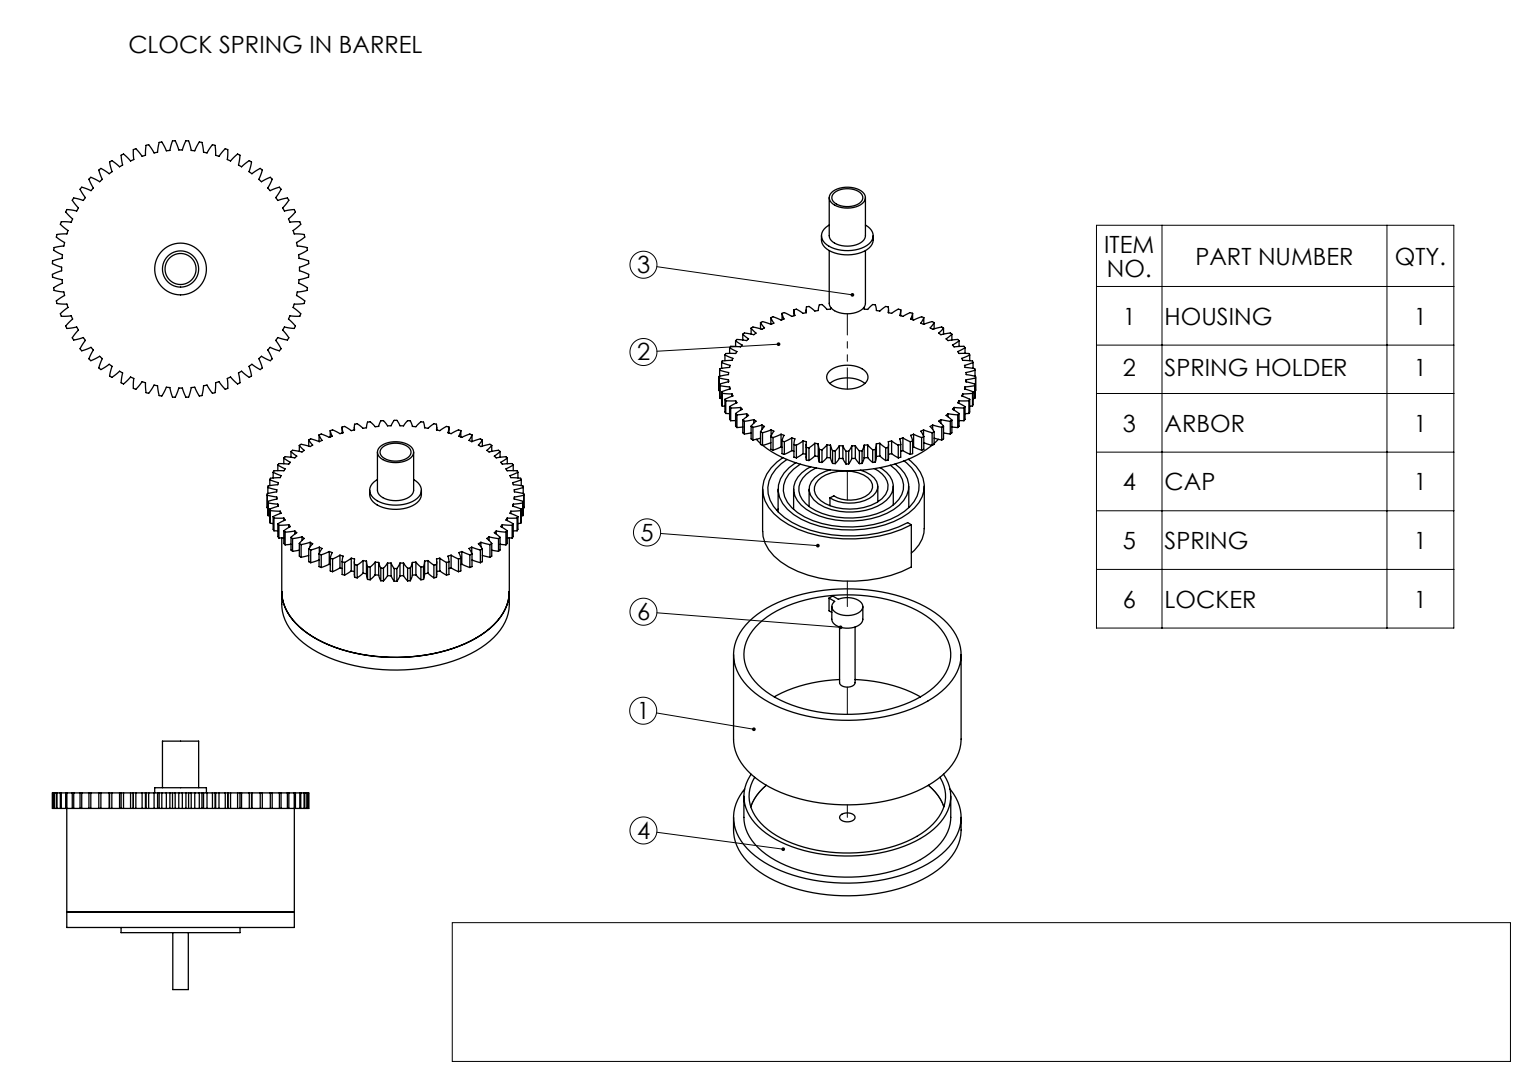
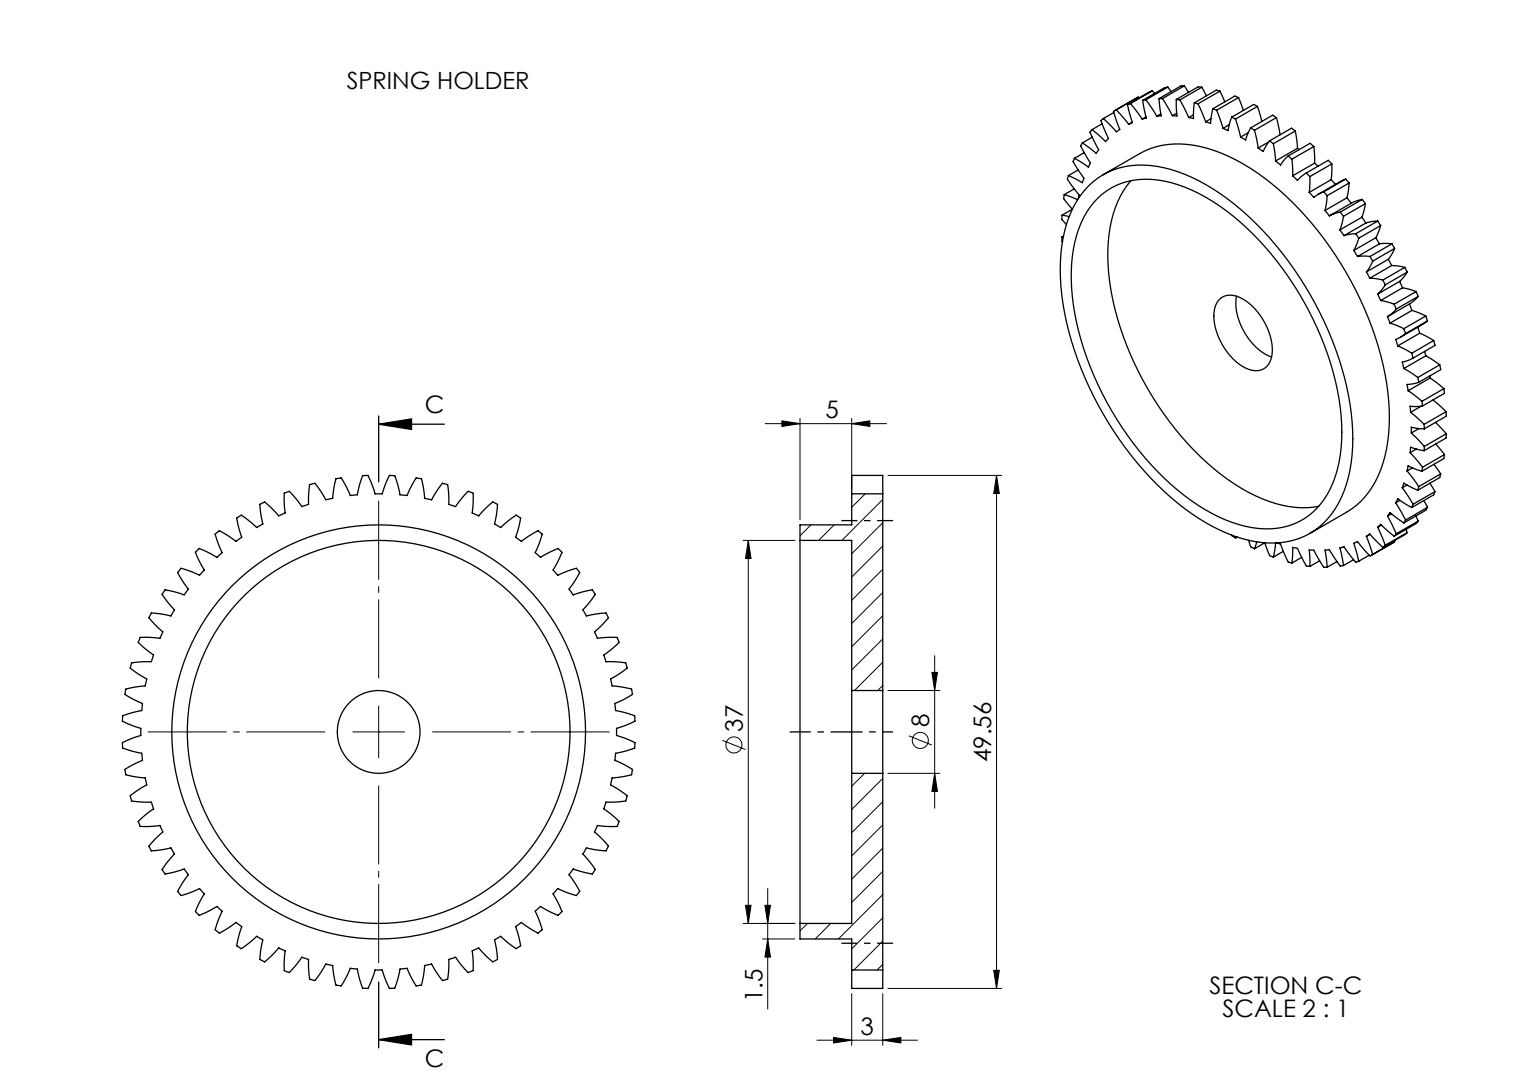
ISO-10303-21;
HEADER;
FILE_DESCRIPTION (('STEP AP214'),
    '1' );
FILE_NAME ('BR-102',
    '2026-10-08T12:30:53',
    ( '' ),
    ( '' ),
    'SwSTEP 2.0',
    'SolidWorks 2026',
    '' );
FILE_SCHEMA (( 'AUTOMOTIVE_DESIGN' ));
ENDSEC;

DATA;
#1 = VECTOR ( 'NONE', #9436, 1000.000000000000000 ) ;
#2 = CARTESIAN_POINT ( 'NONE',  ( 0.000000000000000000, 11.20082935824103565, -20.08719549084853284 ) ) ;
#3 = CIRCLE ( 'NONE', #2554, 9.599999999999994316 ) ;
#4 = ORIENTED_EDGE ( 'NONE', *, *, #1712, .F. ) ;
#5 = CARTESIAN_POINT ( 'NONE',  ( 13.54728169684850414, 0.8932250400876640128, 10.00000000000000000 ) ) ;
#6 = CARTESIAN_POINT ( 'NONE',  ( 3.000000000000000888, -19.29833442572367375, 11.67026512804540950 ) ) ;
#7 = CIRCLE ( 'NONE', #8025, 9.599999999999996092 ) ;
#8 = DIRECTION ( 'NONE',  ( 0.000000000000000000, 0.000000000000000000, 1.000000000000000000 ) ) ;
#9 = AXIS2_PLACEMENT_3D ( 'NONE', #2328, #5147, #7953 ) ;
#10 = DIRECTION ( 'NONE',  ( 0.000000000000000000, 0.000000000000000000, 1.000000000000000000 ) ) ;
#11 = CARTESIAN_POINT ( 'NONE',  ( -13.43906451854578954, -9.301052350413227643, 10.00000000000000000 ) ) ;
#12 = CARTESIAN_POINT ( 'NONE',  ( 8.539395351299290837, 0.2748098766782898217, 6.857782953271941950E-17 ) ) ;
#13 = DIRECTION ( 'NONE',  ( -1.000000000000000000, -0.000000000000000000, -0.000000000000000000 ) ) ;
#14 = CARTESIAN_POINT ( 'NONE',  ( -22.00000000000000000, 0.000000000000000000, 3.000000000000000000 ) ) ;
#15 = EDGE_CURVE ( 'NONE', #3183, #6148, #9804, .T. ) ;
#16 = ORIENTED_EDGE ( 'NONE', *, *, #10840, .T. ) ;
#17 = AXIS2_PLACEMENT_3D ( 'NONE', #6287, #975, #11260 ) ;
#18 = PRODUCT ( 'spring', 'spring', '', ( #10456 ) ) ;
#19 = EDGE_LOOP ( 'NONE', ( #9760, #9661, #8021, #4048 ) ) ;
#20 = AXIS2_PLACEMENT_3D ( 'NONE', #2237, #8791, #3220 ) ;
#21 = MECHANICAL_DESIGN_GEOMETRIC_PRESENTATION_REPRESENTATION (  '', ( #419 ), #8834 ) ;
#22 = ORIENTED_EDGE ( 'NONE', *, *, #6904, .T. ) ;
#23 = CIRCLE ( 'NONE', #4524, 9.599999999999997868 ) ;
#24 = ADVANCED_FACE ( 'NONE', ( #5969 ), #4246, .T. ) ;
#25 = LINE ( 'NONE', #9459, #11094 ) ;
#26 = CARTESIAN_POINT ( 'NONE',  ( 10.50580257846854337, 1.391709641844861123, 10.00000000000000000 ) ) ;
#27 = DIRECTION ( 'NONE',  ( -1.000000000000000000, 0.000000000000000000, -0.000000000000000000 ) ) ;
#28 = DIRECTION ( 'NONE',  ( -1.000000000000000000, 0.000000000000000000, 0.000000000000000000 ) ) ;
#29 = CARTESIAN_POINT ( 'NONE',  ( 3.000000000000000888, 21.14796121233209192, -9.039786367038628256 ) ) ;
#30 = CIRCLE ( 'NONE', #1023, 22.99899999999999878 ) ;
#31 = CARTESIAN_POINT ( 'NONE',  ( 8.800885721068835821, 6.316044917328127895, 3.747395293195558847E-16 ) ) ;
#32 = EDGE_CURVE ( 'NONE', #9019, #7573, #5110, .T. ) ;
#33 = DIRECTION ( 'NONE',  ( 0.000000000000000000, 0.3090169943749479509, -0.9510565162951534202 ) ) ;
#34 = DIRECTION ( 'NONE',  ( 0.000000000000000000, -1.000000000000000000, -1.048062100069321163E-14 ) ) ;
#35 = VERTEX_POINT ( 'NONE', #7865 ) ;
#36 = ORIENTED_EDGE ( 'NONE', *, *, #9803, .F. ) ;
#37 = ORIENTED_EDGE ( 'NONE', *, *, #3148, .F. ) ;
#38 = VECTOR ( 'NONE', #7219, 1000.000000000000000 ) ;
#39 = ORIENTED_EDGE ( 'NONE', *, *, #3079, .T. ) ;
#40 = DIRECTION ( 'NONE',  ( -1.000000000000000000, 0.000000000000000000, 0.000000000000000000 ) ) ;
#41 = AXIS2_PLACEMENT_3D ( 'NONE', #9489, #9312, #7403 ) ;
#42 = DIRECTION ( 'NONE',  ( 0.000000000000000000, 0.000000000000000000, 1.000000000000000000 ) ) ;
#43 = DIRECTION ( 'NONE',  ( -1.000000000000000000, 0.000000000000000000, 0.000000000000000000 ) ) ;
#44 = LINE ( 'NONE', #10212, #8176 ) ;
#45 = CARTESIAN_POINT ( 'NONE',  ( 3.000000000000000888, 0.000000000000000000, 0.000000000000000000 ) ) ;
#46 = CARTESIAN_POINT ( 'NONE',  ( -11.99326810842395474, 8.590522060507202795, 3.747395293195558847E-16 ) ) ;
#47 = DIRECTION ( 'NONE',  ( 0.000000000000000000, 0.000000000000000000, 1.000000000000000000 ) ) ;
#48 = AXIS2_PLACEMENT_3D ( 'NONE', #10892, #6417, #1590 ) ;
#49 = CARTESIAN_POINT ( 'NONE',  ( 0.000000000000000000, -6.168200451485582825, -24.02068490260619171 ) ) ;
#50 = ORIENTED_EDGE ( 'NONE', *, *, #1342, .T. ) ;
#51 = ORIENTED_EDGE ( 'NONE', *, *, #6988, .T. ) ;
#52 = VECTOR ( 'NONE', #9630, 1000.000000000000000 ) ;
#53 = DIRECTION ( 'NONE',  ( -1.000000000000000000, 0.000000000000000000, 0.000000000000000000 ) ) ;
#54 = ORIENTED_EDGE ( 'NONE', *, *, #10768, .T. ) ;
#55 = DIRECTION ( 'NONE',  ( 0.000000000000000000, -0.8090169943749407899, -0.5877852522924822409 ) ) ;
#56 = AXIS2_PLACEMENT_3D ( 'NONE', #9179, #2517, #5398 ) ;
#57 = FACE_OUTER_BOUND ( 'NONE', #11142, .T. ) ;
#58 = EDGE_LOOP ( 'NONE', ( #4252, #3617, #2595, #8061 ) ) ;
#59 = VECTOR ( 'NONE', #9290, 1000.000000000000000 ) ;
#60 = CARTESIAN_POINT ( 'NONE',  ( 0.000000000000000000, 23.05871956130134492, -9.128825345752797915 ) ) ;
#61 = VECTOR ( 'NONE', #2880, 1000.000000000000000 ) ;
#62 = CARTESIAN_POINT ( 'NONE',  ( 1.500000000000000444, 13.72351598154924979, -20.65684170206477788 ) ) ;
#63 = CARTESIAN_POINT ( 'NONE',  ( -6.211147023100844322, 2.816369743025010308, 10.00000000000000000 ) ) ;
#64 = DIRECTION ( 'NONE',  ( -1.000000000000000000, 0.000000000000000000, 0.000000000000000000 ) ) ;
#65 = DIRECTION ( 'NONE',  ( -1.000000000000000000, 0.000000000000000000, 0.000000000000000000 ) ) ;
#66 = AXIS2_PLACEMENT_3D ( 'NONE', #9964, #4339, #1589 ) ;
#67 = VERTEX_POINT ( 'NONE', #3096 ) ;
#68 = DIRECTION ( 'NONE',  ( 0.000000000000000000, 0.3090169943749479509, -0.9510565162951534202 ) ) ;
#69 = ADVANCED_FACE ( 'NONE', ( #8905 ), #11651, .T. ) ;
#70 = EDGE_LOOP ( 'NONE', ( #8780, #11207, #4314, #267 ) ) ;
#71 = EDGE_CURVE ( 'NONE', #10823, #3496, #9699, .T. ) ;
#72 = EDGE_CURVE ( 'NONE', #67, #4226, #10582, .T. ) ;
#73 = CARTESIAN_POINT ( 'NONE',  ( 12.88139461472802516, -9.891864711285373701, 10.00000000000000000 ) ) ;
#74 = DIRECTION ( 'NONE',  ( -1.000000000000000000, 0.000000000000000000, 0.000000000000000000 ) ) ;
#75 = CIRCLE ( 'NONE', #9465, 9.599999999999996092 ) ;
#76 = CARTESIAN_POINT ( 'NONE',  ( 3.000000000000000888, 4.445336973060856955, 22.56530478845650123 ) ) ;
#77 = CARTESIAN_POINT ( 'NONE',  ( 0.000000000000000000, 0.000000000000000000, 0.000000000000000000 ) ) ;
#78 = CARTESIAN_POINT ( 'NONE',  ( -3.251399079312189855, 15.05603916236422890, 10.00000000000000000 ) ) ;
#79 = CARTESIAN_POINT ( 'NONE',  ( 5.267519402444978738, 2.381954139586884622, 6.857782953271941950E-17 ) ) ;
#80 = CYLINDRICAL_SURFACE ( 'NONE', #11012, 24.80000000000000071 ) ;
#81 = EDGE_CURVE ( 'NONE', #3630, #9406, #2177, .T. ) ;
#82 = CARTESIAN_POINT ( 'NONE',  ( 0.000000000000000000, -9.128825345752877851, -23.05871956130131650 ) ) ;
#83 = EDGE_LOOP ( 'NONE', ( #9902, #9745, #3116, #9830 ) ) ;
#84 = LINE ( 'NONE', #11348, #8005 ) ;
#85 = CIRCLE ( 'NONE', #8890, 9.599999999999996092 ) ;
#86 = ORIENTED_EDGE ( 'NONE', *, *, #7277, .F. ) ;
#87 = DIRECTION ( 'NONE',  ( 1.000000000000000000, 0.000000000000000000, 0.000000000000000000 ) ) ;
#88 = CARTESIAN_POINT ( 'NONE',  ( -8.694522232909452697, -2.966707450564700643, 10.00000000000000000 ) ) ;
#89 = FACE_OUTER_BOUND ( 'NONE', #5570, .T. ) ;
#90 = EDGE_CURVE ( 'NONE', #11050, #6456, #8224, .T. ) ;
#91 = CARTESIAN_POINT ( 'NONE',  ( 9.962304844536467030, 3.945508033568876360, 3.747395293195558847E-16 ) ) ;
#92 = DIRECTION ( 'NONE',  ( -1.000000000000000000, 0.000000000000000000, -0.000000000000000000 ) ) ;
#93 = ADVANCED_FACE ( 'NONE', ( #4372 ), #1729, .T. ) ;
#94 = CYLINDRICAL_SURFACE ( 'NONE', #1594, 9.600000000000001421 ) ;
#95 = EDGE_LOOP ( 'NONE', ( #11816, #4327, #9723, #6573 ) ) ;
#96 = ORIENTED_EDGE ( 'NONE', *, *, #6796, .F. ) ;
#97 = EDGE_LOOP ( 'NONE', ( #3670, #7839, #7441, #7336 ) ) ;
#98 = DIRECTION ( 'NONE',  ( -0.000000000000000000, 0.000000000000000000, 1.000000000000000000 ) ) ;
#99 = AXIS2_PLACEMENT_3D ( 'NONE', #9136, #8103, #9261 ) ;
#100 = CYLINDRICAL_SURFACE ( 'NONE', #2958, 9.599999999999997868 ) ;
#101 = EDGE_CURVE ( 'NONE', #2317, #5920, #9198, .T. ) ;
#102 = CARTESIAN_POINT ( 'NONE',  ( 1.500000000000000444, -17.71842311621541555, 17.35216073792434699 ) ) ;
#103 = CARTESIAN_POINT ( 'NONE',  ( 3.000000000000000888, 0.000000000000000000, 0.000000000000000000 ) ) ;
#104 = DIRECTION ( 'NONE',  ( 0.000000000000000000, 0.000000000000000000, 1.000000000000000000 ) ) ;
#105 = CARTESIAN_POINT ( 'NONE',  ( 1.050035089571674352, -12.78847817906846096, 3.747395293195558847E-16 ) ) ;
#106 = ADVANCED_FACE ( 'NONE', ( #7353 ), #11098, .T. ) ;
#107 = CIRCLE ( 'NONE', #4811, 9.599999999999997868 ) ;
#108 = DIRECTION ( 'NONE',  ( 0.000000000000000000, 0.9135454576425990902, 0.4067366430758040385 ) ) ;
#109 = ORIENTED_EDGE ( 'NONE', *, *, #7807, .F. ) ;
#110 = VERTEX_POINT ( 'NONE', #8057 ) ;
#111 = CARTESIAN_POINT ( 'NONE',  ( -10.11701526667144257, 11.92482893257633947, 10.00000000000000000 ) ) ;
#112 = ORIENTED_EDGE ( 'NONE', *, *, #7114, .T. ) ;
#113 = LINE ( 'NONE', #9365, #1823 ) ;
#114 = EDGE_CURVE ( 'NONE', #4536, #8735, #5706, .T. ) ;
#115 = CARTESIAN_POINT ( 'NONE',  ( 3.000000000000000888, -13.79477846460783574, -18.40266524480602683 ) ) ;
#116 = VECTOR ( 'NONE', #1337, 1000.000000000000000 ) ;
#117 = VERTEX_POINT ( 'NONE', #8324 ) ;
#118 = DIRECTION ( 'NONE',  ( -1.000000000000000000, 0.000000000000000000, 0.000000000000000000 ) ) ;
#119 = DIRECTION ( 'NONE',  ( 0.000000000000000000, 0.000000000000000000, 1.000000000000000000 ) ) ;
#120 = CARTESIAN_POINT ( 'NONE',  ( -12.27443204883033623, 3.949650873796764827, 6.857782953271941950E-17 ) ) ;
#121 = CARTESIAN_POINT ( 'NONE',  ( 1.500000000000000444, -19.10918332567968037, 15.80756504416684649 ) ) ;
#122 = LINE ( 'NONE', #10596, #2752 ) ;
#123 = EDGE_LOOP ( 'NONE', ( #5719, #2257, #1328, #877 ) ) ;
#124 = ORIENTED_EDGE ( 'NONE', *, *, #10581, .T. ) ;
#125 = CYLINDRICAL_SURFACE ( 'NONE', #591, 24.80000000000000071 ) ;
#126 = ORIENTED_EDGE ( 'NONE', *, *, #101, .T. ) ;
#127 = CARTESIAN_POINT ( 'NONE',  ( -3.043536693350107569, 14.07442491708026111, 10.00000000000000000 ) ) ;
#128 = DIRECTION ( 'NONE',  ( -1.000000000000000000, -0.000000000000000000, 0.000000000000000000 ) ) ;
#129 = DIRECTION ( 'NONE',  ( -1.000000000000000000, -0.000000000000000000, -0.000000000000000000 ) ) ;
#130 = DIRECTION ( 'NONE',  ( -1.000000000000000000, -0.000000000000000000, -0.000000000000000000 ) ) ;
#131 = CARTESIAN_POINT ( 'NONE',  ( 10.35108484788239203, -9.702746953904565430, 10.00000000000000000 ) ) ;
#132 = CARTESIAN_POINT ( 'NONE',  ( 3.000000000000000888, -20.08719549084857192, -11.20082935824096459 ) ) ;
#133 = DIRECTION ( 'NONE',  ( 0.000000000000000000, 0.000000000000000000, 1.000000000000000000 ) ) ;
#134 = EDGE_CURVE ( 'NONE', #11556, #1082, #8831, .T. ) ;
#135 = CARTESIAN_POINT ( 'NONE',  ( 0.000000000000000000, 23.88662356770124262, -6.668524164681382871 ) ) ;
#136 = EDGE_LOOP ( 'NONE', ( #8153, #10755, #690, #2326 ) ) ;
#137 = CARTESIAN_POINT ( 'NONE',  ( 3.000000000000000888, 23.05871956130122769, 9.128825345753107001 ) ) ;
#138 = ADVANCED_FACE ( 'NONE', ( #8260 ), #9330, .T. ) ;
#139 = VERTEX_POINT ( 'NONE', #6556 ) ;
#140 = AXIS2_PLACEMENT_3D ( 'NONE', #1311, #3213, #4191 ) ;
#141 = DIRECTION ( 'NONE',  ( -1.000000000000000000, 0.000000000000000000, 0.000000000000000000 ) ) ;
#142 = CARTESIAN_POINT ( 'NONE',  ( -8.962830026514758686, 0.7152994853347287574, 10.00000000000000000 ) ) ;
#143 = EDGE_CURVE ( 'NONE', #264, #10120, #7532, .T. ) ;
#144 = CARTESIAN_POINT ( 'NONE',  ( 3.000000000000000888, -19.75591328264893676, 10.87771529938155268 ) ) ;
#145 = EDGE_CURVE ( 'NONE', #6788, #7710, #2973, .T. ) ;
#146 = CARTESIAN_POINT ( 'NONE',  ( -0.1586286459269546645, 8.284426055182338544, 3.747395293195558847E-16 ) ) ;
#147 = CARTESIAN_POINT ( 'NONE',  ( -14.12277927129995803, -8.146689865454474599, 6.857782953271941950E-17 ) ) ;
#148 = EDGE_CURVE ( 'NONE', #2827, #622, #1200, .T. ) ;
#149 = LINE ( 'NONE', #3894, #4131 ) ;
#150 = ORIENTED_EDGE ( 'NONE', *, *, #11407, .F. ) ;
#151 = ORIENTED_EDGE ( 'NONE', *, *, #1050, .T. ) ;
#152 = CARTESIAN_POINT ( 'NONE',  ( 0.000000000000000000, -20.65684170206500170, 13.72351598154890873 ) ) ;
#153 = DIRECTION ( 'NONE',  ( -1.000000000000000000, -0.000000000000000000, -0.000000000000000000 ) ) ;
#154 = ORIENTED_EDGE ( 'NONE', *, *, #10715, .T. ) ;
#155 = CIRCLE ( 'NONE', #8572, 24.80000000000000071 ) ;
#156 = DIRECTION ( 'NONE',  ( 0.000000000000000000, 0.000000000000000000, -1.000000000000000000 ) ) ;
#157 = DIRECTION ( 'NONE',  ( 0.000000000000000000, 0.000000000000000000, 1.000000000000000000 ) ) ;
#158 = AXIS2_PLACEMENT_3D ( 'NONE', #8860, #4204, #7932 ) ;
#159 = DIRECTION ( 'NONE',  ( -1.000000000000000000, 0.000000000000000000, 0.000000000000000000 ) ) ;
#160 = CARTESIAN_POINT ( 'NONE',  ( 4.123629756449401107, -15.38522696314584515, 3.747395293195558847E-16 ) ) ;
#161 = B_SPLINE_CURVE_WITH_KNOTS ( 'NONE', 3,
 ( #5386, #11258, #9477, #10271, #12042, #10215, #12099, #7452, #5566, #5686, #3851, #160, #7515, #4646, #6654, #11313, #9416, #9236, #7383, #10392, #2746, #1763, #2872, #3726, #5623, #6594, #5504, #8321, #3906, #856, #2009, #46, #11199, #4589, #1040, #5753, #1094, #913, #4825, #7630, #10329, #8563, #2815, #11374, #6539, #2994, #9353, #6716, #3663, #11126, #7571, #6477, #4770, #1830, #9296, #3796, #1889, #970, #8381, #4710, #8449, #1947, #8509, #2933, #105, #5808, #11490, #10452, #2070, #5004, #9535, #1151, #7935, #4206, #2189, #4887, #8625, #2303, #3969, #3113, #8687, #225, #10574, #5125, #8800, #6946, #5984, #7698, #11433, #6039, #1391, #1325, #4087, #10690, #4024, #9597, #3053, #3228, #6772, #10509, #9711, #1215, #9768, #2124, #5062, #8863, #11664, #408, #7880, #5865, #4951, #3282, #6828, #5928, #468, #286, #7753, #9657, #1271, #4153, #8742, #2249, #11611, #345, #7815, #11553, #3175, #6894, #10638, #8975, #3350, #11847, #7002, #11906, #8058, #9153, #10749, #585, #7066, #6106, #3533, #7247, #11790, #770, #2367, #4324, #10820, #9840, #11001, #2551, #1450, #528, #2615, #7987, #11723, #8178, #11967, #4444, #2429, #3420, #4261, #4507, #5185, #6350, #5309, #7127, #8920, #10933, #10073, #1692, #6167, #5425, #8243, #4388, #10877, #9895, #7186, #1508, #5243, #2488, #6225, #9952, #1569, #9100, #9042, #6290, #655, #8121, #3476, #10010, #1636, #5374, #710, #8306, #12028, #6526, #1933, #2735, #5669, #3652, #6463, #3595, #7435, #11056, #2671, #7560, #3838, #4633 ),
 .UNSPECIFIED., .F., .F.,
 ( 4, 2, 2, 2, 2, 2, 2, 2, 2, 2, 2, 2, 2, 2, 2, 2, 2, 2, 2, 2, 2, 2, 2, 2, 2, 2, 2, 2, 2, 2, 2, 2, 2, 2, 2, 2, 2, 2, 2, 2, 2, 2, 2, 2, 2, 2, 2, 2, 2, 2, 2, 2, 2, 2, 2, 2, 2, 2, 2, 2, 2, 2, 2, 2, 2, 2, 2, 2, 2, 2, 2, 2, 2, 2, 2, 2, 2, 2, 2, 2, 2, 2, 2, 2, 2, 2, 2, 2, 2, 2, 2, 2, 2, 2, 2, 2, 2, 2, 2, 2, 2, 2, 2, 4 ),
 ( 0.000000000000000000, 0.007812500000000000000, 0.01562500000000000000, 0.02343750000000000000, 0.03125000000000000000, 0.03906250000000000000, 0.04687500000000000000, 0.05468750000000000000, 0.06250000000000000000, 0.07031250000000000000, 0.07812500000000000000, 0.08593750000000000000, 0.09375000000000000000, 0.1015624999999999861, 0.1093750000000000000, 0.1171875000000000000, 0.1250000000000000000, 0.1328125000000000000, 0.1406250000000000000, 0.1484375000000000000, 0.1562500000000000000, 0.1640624999999999722, 0.1718750000000000000, 0.1796875000000000000, 0.1875000000000000000, 0.1953125000000000000, 0.2031249999999999722, 0.2109375000000000000, 0.2187500000000000000, 0.2265625000000000000, 0.2343750000000000000, 0.2421875000000000000, 0.2500000000000000000, 0.2578125000000000000, 0.2656250000000000000, 0.2734375000000000000, 0.2812500000000000000, 0.2890625000000000000, 0.2968750000000000000, 0.3046875000000000000, 0.3125000000000000000, 0.3203125000000000000, 0.3281249999999999445, 0.3359375000000000000, 0.3437500000000000000, 0.3515625000000000000, 0.3593750000000000000, 0.3671874999999999445, 0.3750000000000000000, 0.3828125000000000000, 0.3906250000000000000, 0.3984375000000000000, 0.4062499999999999445, 0.4140625000000000000, 0.4218750000000000000, 0.4296875000000000000, 0.4375000000000000000, 0.4453125000000000000, 0.4531250000000000000, 0.4609375000000000000, 0.4687500000000000000, 0.4765625000000000000, 0.4843750000000000000, 0.4921875000000000000, 0.5000000000000000000, 0.5078125000000000000, 0.5156250000000000000, 0.5234375000000000000, 0.5312500000000000000, 0.5390625000000000000, 0.5468750000000000000, 0.5546875000000000000, 0.5625000000000000000, 0.5703125000000000000, 0.5781250000000000000, 0.5859375000000000000, 0.5937500000000000000, 0.6015625000000000000, 0.6093750000000000000, 0.6171874999999998890, 0.6250000000000000000, 0.6328125000000000000, 0.6406250000000000000, 0.6484375000000000000, 0.6562499999999998890, 0.6640625000000000000, 0.6718750000000000000, 0.6796875000000000000, 0.6875000000000000000, 0.6953124999999998890, 0.7031250000000000000, 0.7109375000000000000, 0.7187500000000000000, 0.7265625000000000000, 0.7343749999999998890, 0.7421875000000000000, 0.7500000000000000000, 0.7656250000000000000, 0.7812500000000000000, 0.7968750000000000000, 0.8124999999999998890, 0.8281250000000000000, 0.8437500000000000000, 0.8499999999999999778 ),
 .UNSPECIFIED. ) ;
#162 = CARTESIAN_POINT ( 'NONE',  ( 0.000000000000000000, 0.000000000000000000, -5.000000000000000000 ) ) ;
#163 = CIRCLE ( 'NONE', #7193, 9.599999999999996092 ) ;
#164 = ORIENTED_EDGE ( 'NONE', *, *, #9086, .T. ) ;
#165 = ORIENTED_EDGE ( 'NONE', *, *, #3483, .F. ) ;
#166 = DIRECTION ( 'NONE',  ( 1.000000000000000000, 0.000000000000000000, 0.000000000000000000 ) ) ;
#167 = CARTESIAN_POINT ( 'NONE',  ( -12.80690425020244128, 9.177692349400032867, 10.00000000000000000 ) ) ;
#168 = ORIENTED_EDGE ( 'NONE', *, *, #4197, .F. ) ;
#169 = CARTESIAN_POINT ( 'NONE',  ( 3.000000000000000888, 11.79560690673872259, 19.74380051311544193 ) ) ;
#170 = EDGE_CURVE ( 'NONE', #8421, #7675, #12083, .T. ) ;
#171 = CARTESIAN_POINT ( 'NONE',  ( 3.000000000000000888, 0.000000000000000000, 0.000000000000000000 ) ) ;
#172 = ORIENTED_EDGE ( 'NONE', *, *, #10346, .T. ) ;
#173 = CIRCLE ( 'NONE', #10738, 9.599999999999997868 ) ;
#174 = DIRECTION ( 'NONE',  ( 0.000000000000000000, 0.000000000000000000, -1.000000000000000000 ) ) ;
#175 = AXIS2_PLACEMENT_3D ( 'NONE', #4264, #7991, #7881 ) ;
#176 = DIRECTION ( 'NONE',  ( 0.000000000000000000, 0.000000000000000000, 1.000000000000000000 ) ) ;
#177 = CARTESIAN_POINT ( 'NONE',  ( -10.84705874452746066, 6.751620637727320684, 6.857782953271941950E-17 ) ) ;
#178 = DIRECTION ( 'NONE',  ( 0.000000000000000000, 0.000000000000000000, 1.000000000000000000 ) ) ;
#179 = EDGE_CURVE ( 'NONE', #5993, #10077, #7445, .T. ) ;
#180 = FACE_BOUND ( 'NONE', #4104, .T. ) ;
#181 = ORIENTED_EDGE ( 'NONE', *, *, #10463, .F. ) ;
#182 = EDGE_LOOP ( 'NONE', ( #7159, #6754, #6114, #7604 ) ) ;
#183 = DIRECTION ( 'NONE',  ( -1.000000000000000000, -0.000000000000000000, 0.000000000000000000 ) ) ;
#184 = ORIENTED_EDGE ( 'NONE', *, *, #4970, .F. ) ;
#185 = CARTESIAN_POINT ( 'NONE',  ( -15.00596061316374197, -1.728743269517114767, 10.00000000000000000 ) ) ;
#186 = CIRCLE ( 'NONE', #2152, 19.00000000000000000 ) ;
#187 = DIRECTION ( 'NONE',  ( 0.000000000000000000, -0.2079116908177466305, -0.9781476007338082423 ) ) ;
#188 = SURFACE_STYLE_USAGE ( .BOTH. , #11225 ) ;
#189 = CARTESIAN_POINT ( 'NONE',  ( 3.000000000000000888, -11.67026512804560134, 19.29833442572355651 ) ) ;
#190 = DIRECTION ( 'NONE',  ( -1.000000000000000000, 0.000000000000000000, 0.000000000000000000 ) ) ;
#191 = CARTESIAN_POINT ( 'NONE',  ( 14.53830338343600559, -0.2437330612273629071, 10.00000000000000000 ) ) ;
#192 = DIRECTION ( 'NONE',  ( -1.000000000000000000, -0.000000000000000000, -0.000000000000000000 ) ) ;
#193 = CARTESIAN_POINT ( 'NONE',  ( 3.000000000000000888, 0.000000000000000000, 0.000000000000000000 ) ) ;
#194 = VECTOR ( 'NONE', #12063, 1000.000000000000000 ) ;
#195 = CARTESIAN_POINT ( 'NONE',  ( 0.000000000000000000, 22.90635393027946165, 2.062268319295641472 ) ) ;
#196 = ORIENTED_EDGE ( 'NONE', *, *, #179, .F. ) ;
#197 =( GEOMETRIC_REPRESENTATION_CONTEXT ( 3 ) GLOBAL_UNCERTAINTY_ASSIGNED_CONTEXT ( ( #10141 ) ) GLOBAL_UNIT_ASSIGNED_CONTEXT ( ( #1001, #11583, #11461 ) ) REPRESENTATION_CONTEXT ( 'NONE', 'WORKASPACE' ) );
#198 = CARTESIAN_POINT ( 'NONE',  ( 0.000000000000000000, 8.753070780933159156, 20.78471918669863427 ) ) ;
#199 = ORIENTED_EDGE ( 'NONE', *, *, #8228, .F. ) ;
#200 = EDGE_LOOP ( 'NONE', ( #985, #7534, #923, #1511 ) ) ;
#201 = FACE_OUTER_BOUND ( 'NONE', #6676, .T. ) ;
#202 = CARTESIAN_POINT ( 'NONE',  ( 2.581500635392915299, -6.456130005640037695, 10.00000000000000000 ) ) ;
#203 = AXIS2_PLACEMENT_3D ( 'NONE', #4845, #183, #3931 ) ;
#204 = AXIS2_PLACEMENT_3D ( 'NONE', #2867, #1942, #9708 ) ;
#205 = CARTESIAN_POINT ( 'NONE',  ( 3.000000000000000888, 3.623565124517108771, 24.53384959170459112 ) ) ;
#206 = CARTESIAN_POINT ( 'NONE',  ( 7.605204090344414247, 4.385345779697003010, 10.00000000000000000 ) ) ;
#207 = EDGE_CURVE ( 'NONE', #11877, #10975, #1592, .T. ) ;
#208 = CARTESIAN_POINT ( 'NONE',  ( -12.06849956494802889, -5.462025159506374017, 6.857782953271941950E-17 ) ) ;
#209 = CARTESIAN_POINT ( 'NONE',  ( 3.000000000000000888, -18.80635025205178579, 13.23915371906949012 ) ) ;
#210 = AXIS2_PLACEMENT_3D ( 'NONE', #11002, #1452, #711 ) ;
#211 = ORIENTED_EDGE ( 'NONE', *, *, #11236, .T. ) ;
#212 = PRESENTATION_LAYER_ASSIGNMENT (  '', '', ( #419 ) ) ;
#213 = EDGE_CURVE ( 'NONE', #1474, #6584, #2468, .T. ) ;
#214 = EDGE_CURVE ( 'NONE', #11471, #12032, #3698, .T. ) ;
#215 = VERTEX_POINT ( 'NONE', #5899 ) ;
#216 = DIRECTION ( 'NONE',  ( 0.000000000000000000, 0.000000000000000000, 1.000000000000000000 ) ) ;
#217 = DIRECTION ( 'NONE',  ( 1.000000000000000000, 0.000000000000000000, 0.000000000000000000 ) ) ;
#218 = EDGE_CURVE ( 'NONE', #5509, #9694, #2903, .T. ) ;
#219 = VERTEX_POINT ( 'NONE', #319 ) ;
#220 = PRODUCT ( 'locker', 'locker', '', ( #5871 ) ) ;
#221 = DIRECTION ( 'NONE',  ( -1.000000000000000000, -0.000000000000000000, -0.000000000000000000 ) ) ;
#222 = CARTESIAN_POINT ( 'NONE',  ( -10.00000000000000000, 0.000000000000000000, 0.000000000000000000 ) ) ;
#223 = VECTOR ( 'NONE', #5078, 1000.000000000000000 ) ;
#224 = LINE ( 'NONE', #3968, #11226 ) ;
#225 = CARTESIAN_POINT ( 'NONE',  ( -10.51222845931327576, 5.388985543800765221, 3.747395293195558847E-16 ) ) ;
#226 = AXIS2_PLACEMENT_3D ( 'NONE', #2459, #9011, #4118 ) ;
#227 = EDGE_CURVE ( 'NONE', #9479, #5646, #2572, .T. ) ;
#228 = DIRECTION ( 'NONE',  ( 0.000000000000000000, 0.000000000000000000, 1.000000000000000000 ) ) ;
#229 = ORIENTED_EDGE ( 'NONE', *, *, #9164, .T. ) ;
#230 = VECTOR ( 'NONE', #10343, 1000.000000000000000 ) ;
#231 = ORIENTED_EDGE ( 'NONE', *, *, #8776, .T. ) ;
#232 = CARTESIAN_POINT ( 'NONE',  ( 0.000000000000000000, 23.00000000000000711, 0.000000000000000000 ) ) ;
#233 = CARTESIAN_POINT ( 'NONE',  ( 4.382127860174852785, -16.35473703246191235, 10.00000000000000000 ) ) ;
#234 = AXIS2_PLACEMENT_3D ( 'NONE', #3106, #10445, #9650 ) ;
#235 = ORIENTED_EDGE ( 'NONE', *, *, #11407, .T. ) ;
#236 = CARTESIAN_POINT ( 'NONE',  ( 3.000000000000000888, -8.753070780933295936, 20.78471918669858098 ) ) ;
#237 = DIRECTION ( 'NONE',  ( 0.000000000000000000, 0.4067366430757948237, 0.9135454576426034201 ) ) ;
#238 = LINE ( 'NONE', #7709, #6766 ) ;
#239 = ORIENTED_EDGE ( 'NONE', *, *, #8409, .T. ) ;
#240 = AXIS2_PLACEMENT_3D ( 'NONE', #2683, #723, #8075 ) ;
#241 = DIRECTION ( 'NONE',  ( -1.000000000000000000, 0.000000000000000000, 0.000000000000000000 ) ) ;
#242 = EDGE_CURVE ( 'NONE', #1657, #5674, #9219, .T. ) ;
#243 = DIRECTION ( 'NONE',  ( -1.000000000000000000, 0.000000000000000000, 0.000000000000000000 ) ) ;
#244 = CARTESIAN_POINT ( 'NONE',  ( 5.334478431285537781, 14.15651896542076749, 6.857782953271941950E-17 ) ) ;
#245 = DIRECTION ( 'NONE',  ( -1.000000000000000000, 0.000000000000000000, 0.000000000000000000 ) ) ;
#246 = VERTEX_POINT ( 'NONE', #5725 ) ;
#247 = ADVANCED_FACE ( 'NONE', ( #4057 ), #3140, .T. ) ;
#248 = DIRECTION ( 'NONE',  ( -1.000000000000000000, -0.000000000000000000, -0.000000000000000000 ) ) ;
#249 = CARTESIAN_POINT ( 'NONE',  ( -10.00000000000000000, 0.000000000000000000, 0.000000000000000000 ) ) ;
#250 = EDGE_LOOP ( 'NONE', ( #5066, #8144, #4716, #4779 ) ) ;
#251 = CIRCLE ( 'NONE', #649, 9.599999999999997868 ) ;
#252 = CARTESIAN_POINT ( 'NONE',  ( -4.793139000956300855, -14.90149022103883247, 10.00000000000000000 ) ) ;
#253 = AXIS2_PLACEMENT_3D ( 'NONE', #6645, #1940, #12036 ) ;
#254 = AXIS2_PLACEMENT_3D ( 'NONE', #9306, #8459, #3858 ) ;
#255 = FACE_OUTER_BOUND ( 'NONE', #5644, .T. ) ;
#256 = EDGE_CURVE ( 'NONE', #3896, #6837, #11173, .T. ) ;
#257 = FACE_OUTER_BOUND ( 'NONE', #4671, .T. ) ;
#258 = DIRECTION ( 'NONE',  ( 0.000000000000000000, 0.000000000000000000, 1.000000000000000000 ) ) ;
#259 = CARTESIAN_POINT ( 'NONE',  ( 7.737545192982512532, 9.111483571581279861, 10.00000000000000000 ) ) ;
#260 = VECTOR ( 'NONE', #5503, 1000.000000000000000 ) ;
#261 = DIRECTION ( 'NONE',  ( -1.000000000000000000, -0.000000000000000000, -0.000000000000000000 ) ) ;
#262 = CARTESIAN_POINT ( 'NONE',  ( -6.423942855642367000, 13.01866063961475461, 3.747395293195558847E-16 ) ) ;
#263 = CYLINDRICAL_SURFACE ( 'NONE', #5092, 24.80000000000000071 ) ;
#264 = VERTEX_POINT ( 'NONE', #6627 ) ;
#265 = DIRECTION ( 'NONE',  ( 0.000000000000000000, 0.000000000000000000, 1.000000000000000000 ) ) ;
#266 = ORIENTED_EDGE ( 'NONE', *, *, #9243, .T. ) ;
#267 = ORIENTED_EDGE ( 'NONE', *, *, #11375, .T. ) ;
#268 = CIRCLE ( 'NONE', #3992, 24.80000000000000071 ) ;
#269 = CARTESIAN_POINT ( 'NONE',  ( 0.000000000000000000, -22.54798042742718422, 0.4575788569251160731 ) ) ;
#270 = CARTESIAN_POINT ( 'NONE',  ( 1.482756436301465808, -6.713508106970953015, 10.00000000000000000 ) ) ;
#271 = CARTESIAN_POINT ( 'NONE',  ( 1.500000000000000444, -23.88662356770119644, 6.668524164681547184 ) ) ;
#272 = CARTESIAN_POINT ( 'NONE',  ( 11.51680056346192593, -0.3781118375584788249, 10.00000000000000000 ) ) ;
#273 = CARTESIAN_POINT ( 'NONE',  ( 1.748316258820581170, 15.14524454193558611, 6.857782953271941950E-17 ) ) ;
#274 = CYLINDRICAL_SURFACE ( 'NONE', #9026, 22.99899999999999878 ) ;
#275 = AXIS2_PLACEMENT_3D ( 'NONE', #77, #3821, #7541 ) ;
#276 = DIRECTION ( 'NONE',  ( -1.000000000000000000, 0.000000000000000000, 0.000000000000000000 ) ) ;
#277 = VERTEX_POINT ( 'NONE', #10360 ) ;
#278 = ORIENTED_EDGE ( 'NONE', *, *, #3169, .T. ) ;
#279 = DIRECTION ( 'NONE',  ( 0.000000000000000000, 0.000000000000000000, 1.000000000000000000 ) ) ;
#280 = CARTESIAN_POINT ( 'NONE',  ( 0.000000000000000000, 0.000000000000000000, 0.000000000000000000 ) ) ;
#281 = CARTESIAN_POINT ( 'NONE',  ( 3.017784444055084503, -16.62017357425735753, 6.857782953271941950E-17 ) ) ;
#282 = CIRCLE ( 'NONE', #3035, 22.99899999999999878 ) ;
#283 = DIRECTION ( 'NONE',  ( 0.000000000000000000, -0.8090169943749526693, 0.5877852522924661427 ) ) ;
#284 = CARTESIAN_POINT ( 'NONE',  ( 0.000000000000000000, -13.23915371906942440, -18.80635025205183197 ) ) ;
#285 = ADVANCED_FACE ( 'NONE', ( #2160 ), #1983, .T. ) ;
#286 = CARTESIAN_POINT ( 'NONE',  ( 0.6578947103914138950, -9.792230064638470566, 3.747395293195558847E-16 ) ) ;
#287 = ADVANCED_FACE ( 'NONE', ( #3086 ), #4921, .T. ) ;
#288 = EDGE_CURVE ( 'NONE', #7265, #6939, #10196, .T. ) ;
#289 = CARTESIAN_POINT ( 'NONE',  ( 3.000000000000000888, 0.000000000000000000, 0.000000000000000000 ) ) ;
#290 = ORIENTED_EDGE ( 'NONE', *, *, #3419, .T. ) ;
#291 = ORIENTED_EDGE ( 'NONE', *, *, #1715, .T. ) ;
#292 = APPLICATION_PROTOCOL_DEFINITION ( 'draft international standard', 'automotive_design', 1998, #6763 ) ;
#293 = CARTESIAN_POINT ( 'NONE',  ( -15.56595607421884075, -4.438723023272252988, 10.00000000000000000 ) ) ;
#294 = ORIENTED_EDGE ( 'NONE', *, *, #2175, .F. ) ;
#295 = DIRECTION ( 'NONE',  ( -1.000000000000000000, 0.000000000000000000, -0.000000000000000000 ) ) ;
#296 = CARTESIAN_POINT ( 'NONE',  ( 0.000000000000000000, -17.31945870441157354, 15.13242714128113775 ) ) ;
#297 = LINE ( 'NONE', #4096, #116 ) ;
#298 = ORIENTED_EDGE ( 'NONE', *, *, #7745, .F. ) ;
#299 = EDGE_CURVE ( 'NONE', #7150, #10349, #8718, .T. ) ;
#300 = DIRECTION ( 'NONE',  ( 0.000000000000000000, 0.000000000000000000, 1.000000000000000000 ) ) ;
#301 = AXIS2_PLACEMENT_3D ( 'NONE', #4366, #4615, #5408 ) ;
#302 = MANIFOLD_SOLID_BREP ( 'Extrude-Thin1', #3949 ) ;
#303 = EDGE_CURVE ( 'NONE', #9360, #3895, #826, .T. ) ;
#304 = CARTESIAN_POINT ( 'NONE',  ( 3.000000000000000888, 20.41249101028211754, 9.589108953447965433 ) ) ;
#305 = CARTESIAN_POINT ( 'NONE',  ( -3.251399079312188078, 15.05603916236422180, 6.857782953271941950E-17 ) ) ;
#306 = ORIENTED_EDGE ( 'NONE', *, *, #3487, .F. ) ;
#307 = FACE_OUTER_BOUND ( 'NONE', #8234, .T. ) ;
#308 = VERTEX_POINT ( 'NONE', #2045 ) ;
#309 = CARTESIAN_POINT ( 'NONE',  ( 3.000000000000000888, 4.135161237383916166, -24.45282072769596482 ) ) ;
#310 = ORIENTED_EDGE ( 'NONE', *, *, #6297, .T. ) ;
#311 = AXIS2_PLACEMENT_3D ( 'NONE', #3561, #11026, #9176 ) ;
#312 = CARTESIAN_POINT ( 'NONE',  ( 4.071483724746832067, 10.33449570568845211, 10.00000000000000000 ) ) ;
#313 = CARTESIAN_POINT ( 'NONE',  ( 0.000000000000000000, 0.000000000000000000, 20.00000000000000000 ) ) ;
#314 =( NAMED_UNIT ( * ) PLANE_ANGLE_UNIT ( ) SI_UNIT ( $, .RADIAN. ) );
#315 = CARTESIAN_POINT ( 'NONE',  ( 3.000000000000000888, 23.24434456306336827, -8.645255683528764834 ) ) ;
#316 = FACE_OUTER_BOUND ( 'NONE', #11315, .T. ) ;
#317 = CARTESIAN_POINT ( 'NONE',  ( 12.58137556868281237, 7.823023050435613968, 10.00000000000000000 ) ) ;
#318 = CIRCLE ( 'NONE', #8142, 9.599999999999997868 ) ;
#319 = CARTESIAN_POINT ( 'NONE',  ( 3.000000000000000888, 13.23915371906980276, -18.80635025205156552 ) ) ;
#320 = DIRECTION ( 'NONE',  ( -1.000000000000000000, 0.000000000000000000, 0.000000000000000000 ) ) ;
#321 = CARTESIAN_POINT ( 'NONE',  ( 0.000000000000000000, 0.000000000000000000, 20.00000000000000000 ) ) ;
#322 = CARTESIAN_POINT ( 'NONE',  ( 3.000000000000000888, 5.117118920208799437, -22.42251312757874260 ) ) ;
#323 = ADVANCED_BREP_SHAPE_REPRESENTATION ( '', ( #302, #8474 ), #6316 ) ;
#324 = ORIENTED_EDGE ( 'NONE', *, *, #7929, .F. ) ;
#325 = PRODUCT_DEFINITION_SHAPE ( 'NONE', 'NONE',  #10691 ) ;
#326 = ORIENTED_EDGE ( 'NONE', *, *, #7918, .T. ) ;
#327 = ORIENTED_EDGE ( 'NONE', *, *, #10763, .F. ) ;
#328 = CARTESIAN_POINT ( 'NONE',  ( 0.000000000000000000, 21.97702544527757951, 6.779701584702809924 ) ) ;
#329 = CARTESIAN_POINT ( 'NONE',  ( -0.7379871813790722657, -6.677365878963855472, 10.00000000000000000 ) ) ;
#330 = EDGE_CURVE ( 'NONE', #10333, #8749, #6479, .T. ) ;
#331 = CARTESIAN_POINT ( 'NONE',  ( 0.000000000000000000, 0.000000000000000000, 20.00000000000000000 ) ) ;
#332 = DIRECTION ( 'NONE',  ( 0.000000000000000000, 0.2079116908177532086, 0.9781476007338069101 ) ) ;
#333 = CARTESIAN_POINT ( 'NONE',  ( -8.201440678128605555, 5.289679325232168772, 10.00000000000000000 ) ) ;
#334 = CARTESIAN_POINT ( 'NONE',  ( -15.59049818040117152, 3.373450308083002724, 6.857782953271941950E-17 ) ) ;
#335 = CARTESIAN_POINT ( 'NONE',  ( 3.000000000000000888, 1.901833551798254973, 22.47229024614977888 ) ) ;
#336 = AXIS2_PLACEMENT_3D ( 'NONE', #2470, #6710, #4945 ) ;
#337 = ORIENTED_EDGE ( 'NONE', *, *, #10319, .T. ) ;
#338 = EDGE_CURVE ( 'NONE', #6397, #4410, #2384, .T. ) ;
#339 = AXIS2_PLACEMENT_3D ( 'NONE', #331, #5047, #8783 ) ;
#340 = ORIENTED_EDGE ( 'NONE', *, *, #11523, .F. ) ;
#341 = CARTESIAN_POINT ( 'NONE',  ( 1.499999999999999556, 6.668524164681631561, 23.88662356770117512 ) ) ;
#342 = CARTESIAN_POINT ( 'NONE',  ( 7.795318149608632119, -14.02504990430958998, 10.00000000000000000 ) ) ;
#343 = CARTESIAN_POINT ( 'NONE',  ( 3.000000000000000888, -21.30300407174357957, -7.402892494506506438 ) ) ;
#344 = VECTOR ( 'NONE', #10356, 1000.000000000000000 ) ;
#345 = CARTESIAN_POINT ( 'NONE',  ( -7.402161455537873636, -5.702533393948970186, 3.747395293195558847E-16 ) ) ;
#346 = CARTESIAN_POINT ( 'NONE',  ( -10.00000000000000000, 0.000000000000000000, 0.000000000000000000 ) ) ;
#347 = ORIENTED_EDGE ( 'NONE', *, *, #481, .T. ) ;
#348 = VERTEX_POINT ( 'NONE', #6979 ) ;
#349 = CARTESIAN_POINT ( 'NONE',  ( 17.46093749967478814, -1.431715403549062904, 10.00000000000000000 ) ) ;
#350 = ORIENTED_EDGE ( 'NONE', *, *, #2639, .T. ) ;
#351 = VECTOR ( 'NONE', #11431, 1000.000000000000000 ) ;
#352 = VECTOR ( 'NONE', #8492, 1000.000000000000000 ) ;
#353 = CARTESIAN_POINT ( 'NONE',  ( 0.000000000000000000, 1.556492618230641556, 24.75110766671652485 ) ) ;
#354 = FACE_OUTER_BOUND ( 'NONE', #7228, .T. ) ;
#355 = CARTESIAN_POINT ( 'NONE',  ( 0.000000000000000000, -24.45282072769603587, 4.135161237383499611 ) ) ;
#356 = ORIENTED_EDGE ( 'NONE', *, *, #1238, .T. ) ;
#357 = DIRECTION ( 'NONE',  ( 0.000000000000000000, 0.000000000000000000, 1.000000000000000000 ) ) ;
#358 = CARTESIAN_POINT ( 'NONE',  ( 0.000000000000000000, 0.000000000000000000, 0.000000000000000000 ) ) ;
#359 = CARTESIAN_POINT ( 'NONE',  ( -2.240087900411201982, -13.53314956822677928, 6.857782953271941950E-17 ) ) ;
#360 = AXIS2_PLACEMENT_3D ( 'NONE', #8241, #708, #9894 ) ;
#361 = EDGE_CURVE ( 'NONE', #5937, #3303, #11757, .T. ) ;
#362 = VECTOR ( 'NONE', #11355, 1000.000000000000000 ) ;
#363 = VERTEX_POINT ( 'NONE', #2521 ) ;
#364 = CARTESIAN_POINT ( 'NONE',  ( 0.000000000000000000, 11.02759168516775112, -22.21333432029552668 ) ) ;
#365 = EDGE_LOOP ( 'NONE', ( #9600, #8679, #4955, #8031 ) ) ;
#366 = DIRECTION ( 'NONE',  ( 0.000000000000000000, 0.000000000000000000, 1.000000000000000000 ) ) ;
#367 = ORIENTED_EDGE ( 'NONE', *, *, #6608, .F. ) ;
#368 = EDGE_CURVE ( 'NONE', #8212, #1454, #10724, .T. ) ;
#369 = CARTESIAN_POINT ( 'NONE',  ( -4.046710180314750716, 10.72208681399755648, 10.00000000000000000 ) ) ;
#370 = EDGE_CURVE ( 'NONE', #4413, #11133, #1604, .T. ) ;
#371 = AXIS2_PLACEMENT_3D ( 'NONE', #4586, #7316, #10140 ) ;
#372 = CARTESIAN_POINT ( 'NONE',  ( 0.000000000000000000, 4.135161237383582211, 24.45282072769602166 ) ) ;
#373 = ADVANCED_FACE ( 'NONE', ( #8027 ), #499, .T. ) ;
#374 =( LENGTH_UNIT ( ) NAMED_UNIT ( * ) SI_UNIT ( .MILLI., .METRE. ) );
#375 = DIRECTION ( 'NONE',  ( 0.000000000000000000, 0.000000000000000000, 1.000000000000000000 ) ) ;
#376 = DIRECTION ( 'NONE',  ( -1.000000000000000000, 0.000000000000000000, -0.000000000000000000 ) ) ;
#377 = CARTESIAN_POINT ( 'NONE',  ( 2.259453438922059298, -13.68937604509904737, 10.00000000000000000 ) ) ;
#378 = DIRECTION ( 'NONE',  ( 0.000000000000000000, 0.8090169943749446757, 0.5877852522924770229 ) ) ;
#379 = CARTESIAN_POINT ( 'NONE',  ( -11.21689850597007343, 9.520844388990626683, 3.747395293195558847E-16 ) ) ;
#380 = CIRCLE ( 'NONE', #7211, 9.599999999999997868 ) ;
#381 = CARTESIAN_POINT ( 'NONE',  ( 3.000000000000000888, -19.29833442572351743, -11.67026512804567062 ) ) ;
#382 = ORIENTED_EDGE ( 'NONE', *, *, #1494, .F. ) ;
#383 = DIRECTION ( 'NONE',  ( -1.000000000000000000, 0.000000000000000000, -0.000000000000000000 ) ) ;
#384 = VERTEX_POINT ( 'NONE', #4238 ) ;
#385 = ORIENTED_EDGE ( 'NONE', *, *, #2810, .T. ) ;
#386 = CYLINDRICAL_SURFACE ( 'NONE', #2254, 24.80000000000000071 ) ;
#387 = AXIS2_PLACEMENT_3D ( 'NONE', #6705, #11603, #6819 ) ;
#388 = CARTESIAN_POINT ( 'NONE',  ( 3.000000000000000888, 13.23915371906980276, -18.80635025205156552 ) ) ;
#389 = VECTOR ( 'NONE', #4390, 1000.000000000000000 ) ;
#390 = DIRECTION ( 'NONE',  ( 0.000000000000000000, 0.000000000000000000, 1.000000000000000000 ) ) ;
#391 = CARTESIAN_POINT ( 'NONE',  ( -6.589974825828277538, 7.038139701356666222, 10.00000000000000000 ) ) ;
#392 = EDGE_CURVE ( 'NONE', #2895, #2526, #5317, .T. ) ;
#393 = CARTESIAN_POINT ( 'NONE',  ( -12.72059027619867244, -3.407653011835690471, 6.857782953271941950E-17 ) ) ;
#394 = DIRECTION ( 'NONE',  ( 0.000000000000000000, 0.000000000000000000, 1.000000000000000000 ) ) ;
#395 = FACE_OUTER_BOUND ( 'NONE', #5803, .T. ) ;
#396 = EDGE_LOOP ( 'NONE', ( #8402, #10334, #7110, #9558 ) ) ;
#397 = ADVANCED_FACE ( 'NONE', ( #6257 ), #7100, .T. ) ;
#398 = EDGE_LOOP ( 'NONE', ( #9542, #6481, #3860, #9440 ) ) ;
#399 = AXIS2_PLACEMENT_3D ( 'NONE', #1152, #3055, #3114 ) ;
#400 = VECTOR ( 'NONE', #4611, 1000.000000000000000 ) ;
#401 = VERTEX_POINT ( 'NONE', #1423 ) ;
#402 = CARTESIAN_POINT ( 'NONE',  ( 3.000000000000000888, 0.000000000000000000, 0.000000000000000000 ) ) ;
#403 = CARTESIAN_POINT ( 'NONE',  ( 1.500000000000000222, 0.000000000000000000, 0.000000000000000000 ) ) ;
#404 = LINE ( 'NONE', #8798, #9929 ) ;
#405 = ADVANCED_FACE ( 'NONE', ( #11588 ), #2280, .T. ) ;
#406 = AXIS2_PLACEMENT_3D ( 'NONE', #10470, #10347, #9556 ) ;
#407 = VECTOR ( 'NONE', #6673, 1000.000000000000000 ) ;
#408 = CARTESIAN_POINT ( 'NONE',  ( 8.913847851857145344, -5.129921849437907078, 3.747395293195558847E-16 ) ) ;
#409 = CARTESIAN_POINT ( 'NONE',  ( 0.000000000000000000, 21.30300407174352983, 7.402892494506653875 ) ) ;
#410 = ORIENTED_EDGE ( 'NONE', *, *, #9951, .F. ) ;
#411 = VERTEX_POINT ( 'NONE', #3260 ) ;
#412 = APPLICATION_PROTOCOL_DEFINITION ( 'draft international standard', 'automotive_design', 1998, #2155 ) ;
#413 = CARTESIAN_POINT ( 'NONE',  ( -8.799721882313775723, 9.100398320382247164, 10.00000000000000000 ) ) ;
#414 = AXIS2_PLACEMENT_3D ( 'NONE', #1180, #192, #2968 ) ;
#415 = ORIENTED_EDGE ( 'NONE', *, *, #705, .F. ) ;
#416 = AXIS2_PLACEMENT_3D ( 'NONE', #3272, #11655, #4436 ) ;
#417 = DIRECTION ( 'NONE',  ( 0.000000000000000000, 0.6691306063588544628, 0.7431448254773976858 ) ) ;
#418 = CARTESIAN_POINT ( 'NONE',  ( 1.500000000000000444, -15.80756504416678432, -19.10918332567973721 ) ) ;
#419 = STYLED_ITEM ( 'NONE', ( #8733 ), #4375 ) ;
#420 = CARTESIAN_POINT ( 'NONE',  ( 3.000000000000000888, 18.51065745848395849, -12.88318129270159673 ) ) ;
#421 = EDGE_LOOP ( 'NONE', ( #1532, #5869, #9678, #9526 ) ) ;
#422 = FACE_OUTER_BOUND ( 'NONE', #7887, .T. ) ;
#423 = CYLINDRICAL_SURFACE ( 'NONE', #5915, 9.599999999999997868 ) ;
#424 = CARTESIAN_POINT ( 'NONE',  ( -9.352287007201468327, 3.176141031410556703, 6.857782953271941950E-17 ) ) ;
#425 = CIRCLE ( 'NONE', #7256, 9.599999999999997868 ) ;
#426 = EDGE_LOOP ( 'NONE', ( #4660, #3753, #2493, #2371 ) ) ;
#427 = DIRECTION ( 'NONE',  ( 1.000000000000000000, 0.000000000000000000, 0.000000000000000000 ) ) ;
#428 = DIRECTION ( 'NONE',  ( -1.000000000000000000, 0.000000000000000000, 0.000000000000000000 ) ) ;
#429 = VERTEX_POINT ( 'NONE', #7852 ) ;
#430 = CARTESIAN_POINT ( 'NONE',  ( -8.984113827416489784, -1.502549133976348816, 10.00000000000000000 ) ) ;
#431 =( GEOMETRIC_REPRESENTATION_CONTEXT ( 3 ) GLOBAL_UNCERTAINTY_ASSIGNED_CONTEXT ( ( #7196 ) ) GLOBAL_UNIT_ASSIGNED_CONTEXT ( ( #3634, #3937, #4674 ) ) REPRESENTATION_CONTEXT ( 'NONE', 'WORKASPACE' ) );
#432 = ORIENTED_EDGE ( 'NONE', *, *, #9829, .T. ) ;
#433 = DIRECTION ( 'NONE',  ( 0.000000000000000000, -0.5877852522924633671, -0.8090169943749546677 ) ) ;
#434 = SURFACE_STYLE_USAGE ( .BOTH. , #4112 ) ;
#435 = ORIENTED_EDGE ( 'NONE', *, *, #4714, .F. ) ;
#436 = AXIS2_PLACEMENT_3D ( 'NONE', #4702, #11192, #1883 ) ;
#437 = FACE_OUTER_BOUND ( 'NONE', #11878, .T. ) ;
#438 = CARTESIAN_POINT ( 'NONE',  ( 3.000000000000000888, 22.90635393027946165, 2.062268319295641472 ) ) ;
#439 = CARTESIAN_POINT ( 'NONE',  ( 3.343943643650761022, -10.41127694127790271, 10.00000000000000000 ) ) ;
#440 = DIRECTION ( 'NONE',  ( -1.000000000000000000, 0.000000000000000000, 0.000000000000000000 ) ) ;
#441 = DIRECTION ( 'NONE',  ( 0.000000000000000000, 0.000000000000000000, 1.000000000000000000 ) ) ;
#442 = EDGE_CURVE ( 'NONE', #12032, #9479, #5517, .T. ) ;
#443 = DIRECTION ( 'NONE',  ( 0.000000000000000000, -0.9135454576425964257, -0.4067366430758104223 ) ) ;
#444 = EDGE_CURVE ( 'NONE', #5746, #5082, #6868, .T. ) ;
#445 = ADVANCED_FACE ( 'NONE', ( #6142 ), #5277, .T. ) ;
#446 = DIRECTION ( 'NONE',  ( 0.000000000000000000, 0.000000000000000000, 1.000000000000000000 ) ) ;
#447 = ORIENTED_EDGE ( 'NONE', *, *, #11363, .T. ) ;
#448 = AXIS2_PLACEMENT_3D ( 'NONE', #5250, #7314, #11062 ) ;
#449 = CIRCLE ( 'NONE', #2608, 24.80000000000000071 ) ;
#450 = FACE_OUTER_BOUND ( 'NONE', #3951, .T. ) ;
#451 = AXIS2_PLACEMENT_3D ( 'NONE', #7259, #6360, #5257 ) ;
#452 = DIRECTION ( 'NONE',  ( 0.000000000000000000, 0.000000000000000000, 1.000000000000000000 ) ) ;
#453 = CARTESIAN_POINT ( 'NONE',  ( 3.000000000000000888, -21.96011696265487600, -5.135568396240250522 ) ) ;
#454 = CARTESIAN_POINT ( 'NONE',  ( 5.893263639827395650, 6.717612500730409941, 10.00000000000000000 ) ) ;
#455 = EDGE_CURVE ( 'NONE', #11607, #3718, #7156, .T. ) ;
#456 = CARTESIAN_POINT ( 'NONE',  ( 5.343773788080180331, 10.82393792025543711, 6.857782953271941950E-17 ) ) ;
#457 = DIRECTION ( 'NONE',  ( 0.000000000000000000, 0.9945218953682729568, 0.1045284632676570929 ) ) ;
#458 = ORIENTED_EDGE ( 'NONE', *, *, #10391, .F. ) ;
#459 = ORIENTED_EDGE ( 'NONE', *, *, #4936, .T. ) ;
#460 = AXIS2_PLACEMENT_3D ( 'NONE', #4853, #130, #7598 ) ;
#461 = ORIENTED_EDGE ( 'NONE', *, *, #10996, .F. ) ;
#462 = EDGE_CURVE ( 'NONE', #4079, #6675, #6924, .T. ) ;
#463 = DIRECTION ( 'NONE',  ( 0.000000000000000000, 0.000000000000000000, -1.000000000000000000 ) ) ;
#464 = CARTESIAN_POINT ( 'NONE',  ( 3.000000000000000888, 0.000000000000000000, 0.000000000000000000 ) ) ;
#465 = DIRECTION ( 'NONE',  ( 1.000000000000000000, 0.000000000000000000, 0.000000000000000000 ) ) ;
#466 = EDGE_CURVE ( 'NONE', #3254, #10253, #9814, .T. ) ;
#467 = AXIS2_PLACEMENT_3D ( 'NONE', #3579, #2656, #5467 ) ;
#468 = CARTESIAN_POINT ( 'NONE',  ( 2.257301671556970479, -9.631158585656898197, 3.747395293195558847E-16 ) ) ;
#469 = CYLINDRICAL_SURFACE ( 'NONE', #4322, 9.599999999999997868 ) ;
#470 = DIRECTION ( 'NONE',  ( 0.000000000000000000, 0.000000000000000000, 1.000000000000000000 ) ) ;
#471 = EDGE_LOOP ( 'NONE', ( #5188, #8628, #9006, #4978 ) ) ;
#472 = EDGE_LOOP ( 'NONE', ( #11221, #8128, #9957, #11135 ) ) ;
#473 = CARTESIAN_POINT ( 'NONE',  ( 14.27634331491212549, 3.322769473269123974, 10.00000000000000000 ) ) ;
#474 = VERTEX_POINT ( 'NONE', #9742 ) ;
#475 = AXIS2_PLACEMENT_3D ( 'NONE', #3137, #5034, #6011 ) ;
#476 = DIRECTION ( 'NONE',  ( -1.000000000000000000, 0.000000000000000000, -0.000000000000000000 ) ) ;
#477 = DIRECTION ( 'NONE',  ( 0.000000000000000000, 0.000000000000000000, -1.000000000000000000 ) ) ;
#478 = UNCERTAINTY_MEASURE_WITH_UNIT (LENGTH_MEASURE( 1.000000000000000082E-05 ), #5286, 'distance_accuracy_value', 'NONE');
#479 = CARTESIAN_POINT ( 'NONE',  ( 0.000000000000000000, 0.000000000000000000, -15.00000000000000000 ) ) ;
#480 = EDGE_LOOP ( 'NONE', ( #9305, #6355, #6678, #2511 ) ) ;
#481 = EDGE_CURVE ( 'NONE', #7424, #4541, #1360, .T. ) ;
#482 = DIRECTION ( 'NONE',  ( 0.000000000000000000, 0.000000000000000000, 1.000000000000000000 ) ) ;
#483 = MANIFOLD_SOLID_BREP ( 'Boss-Extrude1', #814 ) ;
#484 = CARTESIAN_POINT ( 'NONE',  ( -4.500000000000000888, 3.903127820947816751E-15, 0.000000000000000000 ) ) ;
#485 = CARTESIAN_POINT ( 'NONE',  ( -8.201440678127905670, 5.289679325232165219, 6.857782953271941950E-17 ) ) ;
#486 = LINE ( 'NONE', #7085, #10595 ) ;
#487 = ORIENTED_EDGE ( 'NONE', *, *, #7990, .F. ) ;
#488 = FACE_OUTER_BOUND ( 'NONE', #6997, .T. ) ;
#489 = ADVANCED_FACE ( 'NONE', ( #686 ), #1482, .F. ) ;
#490 = VERTEX_POINT ( 'NONE', #11216 ) ;
#491 = CARTESIAN_POINT ( 'NONE',  ( -10.00031051369627200, 6.213292778947749007, 10.00000000000000000 ) ) ;
#492 = ORIENTED_EDGE ( 'NONE', *, *, #5461, .F. ) ;
#493 = DIRECTION ( 'NONE',  ( 0.000000000000000000, 0.000000000000000000, 1.000000000000000000 ) ) ;
#494 = CIRCLE ( 'NONE', #6752, 9.599999999999997868 ) ;
#495 = ORIENTED_EDGE ( 'NONE', *, *, #6230, .F. ) ;
#496 = DIRECTION ( 'NONE',  ( -1.000000000000000000, -0.000000000000000000, -0.000000000000000000 ) ) ;
#497 = DIRECTION ( 'NONE',  ( 0.000000000000000000, 0.000000000000000000, 1.000000000000000000 ) ) ;
#498 = CARTESIAN_POINT ( 'NONE',  ( -4.368568794346924022, -9.638580752213403713, 10.00000000000000000 ) ) ;
#499 = CYLINDRICAL_SURFACE ( 'NONE', #3358, 9.599999999999997868 ) ;
#500 = CARTESIAN_POINT ( 'NONE',  ( -11.74902089294173457, -3.156991809147609906, 3.747395293195558847E-16 ) ) ;
#501 = DIRECTION ( 'NONE',  ( 0.000000000000000000, 0.000000000000000000, -1.000000000000000000 ) ) ;
#502 = AXIS2_PLACEMENT_3D ( 'NONE', #6, #11283, #6621 ) ;
#503 = ORIENTED_EDGE ( 'NONE', *, *, #2058, .T. ) ;
#504 = CYLINDRICAL_SURFACE ( 'NONE', #8992, 9.599999999999997868 ) ;
#505 = VERTEX_POINT ( 'NONE', #1848 ) ;
#506 = DIRECTION ( 'NONE',  ( 0.000000000000000000, 0.000000000000000000, 1.000000000000000000 ) ) ;
#507 = ORIENTED_EDGE ( 'NONE', *, *, #11003, .T. ) ;
#508 = LINE ( 'NONE', #10676, #10897 ) ;
#509 = CIRCLE ( 'NONE', #3249, 9.599999999999996092 ) ;
#510 = EDGE_CURVE ( 'NONE', #9078, #5271, #30, .T. ) ;
#511 = DIRECTION ( 'NONE',  ( -1.000000000000000000, -0.000000000000000000, 0.000000000000000000 ) ) ;
#512 = DIRECTION ( 'NONE',  ( -1.000000000000000000, 0.000000000000000000, 0.000000000000000000 ) ) ;
#513 = CARTESIAN_POINT ( 'NONE',  ( 2.919619825260427071, -7.400844473264730716, 10.00000000000000000 ) ) ;
#514 = CARTESIAN_POINT ( 'NONE',  ( -3.909826107002860596, 8.641065831729461522, 6.857782953271941950E-17 ) ) ;
#515 = CARTESIAN_POINT ( 'NONE',  ( 0.000000000000000000, 0.000000000000000000, 0.000000000000000000 ) ) ;
#516 = CARTESIAN_POINT ( 'NONE',  ( 3.000000000000000888, 0.000000000000000000, 0.000000000000000000 ) ) ;
#517 = ADVANCED_FACE ( 'NONE', ( #7468 ), #9254, .T. ) ;
#518 = VERTEX_POINT ( 'NONE', #10288 ) ;
#519 = EDGE_LOOP ( 'NONE', ( #2423, #3597, #5919, #11454 ) ) ;
#520 = ORIENTED_EDGE ( 'NONE', *, *, #9304, .T. ) ;
#521 = ADVANCED_FACE ( 'NONE', ( #8150 ), #5453, .T. ) ;
#522 = CARTESIAN_POINT ( 'NONE',  ( -15.00596061316374197, -1.728743269517114767, 10.00000000000000000 ) ) ;
#523 = EDGE_CURVE ( 'NONE', #2005, #11061, #9418, .T. ) ;
#524 = EDGE_LOOP ( 'NONE', ( #7250, #3552, #2179, #11969 ) ) ;
#525 = CARTESIAN_POINT ( 'NONE',  ( 3.000000000000000888, 0.000000000000000000, 0.000000000000000000 ) ) ;
#526 = FACE_OUTER_BOUND ( 'NONE', #10762, .T. ) ;
#527 = ADVANCED_FACE ( 'NONE', ( #5522 ), #9076, .T. ) ;
#528 = CARTESIAN_POINT ( 'NONE',  ( 7.195390336726608105, 2.736402267197653337, 3.747395293195558847E-16 ) ) ;
#529 = DIRECTION ( 'NONE',  ( -1.000000000000000000, 0.000000000000000000, -0.000000000000000000 ) ) ;
#530 = CARTESIAN_POINT ( 'NONE',  ( 0.000000000000000000, 22.15038895030654942, -4.240409074143872914 ) ) ;
#531 = VERTEX_POINT ( 'NONE', #10047 ) ;
#532 = VERTEX_POINT ( 'NONE', #3683 ) ;
#533 = CARTESIAN_POINT ( 'NONE',  ( -11.61414229320030778, -6.453515506896109422, 10.00000000000000000 ) ) ;
#534 = ORIENTED_EDGE ( 'NONE', *, *, #6875, .F. ) ;
#535 = DIRECTION ( 'NONE',  ( 0.000000000000000000, 0.000000000000000000, 1.000000000000000000 ) ) ;
#536 = DIRECTION ( 'NONE',  ( 0.000000000000000000, 0.000000000000000000, 1.000000000000000000 ) ) ;
#537 = CARTESIAN_POINT ( 'NONE',  ( 3.000000000000000888, 0.000000000000000000, 0.000000000000000000 ) ) ;
#538 = AXIS2_PLACEMENT_3D ( 'NONE', #5653, #6744, #4617 ) ;
#539 = FACE_OUTER_BOUND ( 'NONE', #10644, .T. ) ;
#540 = ORIENTED_EDGE ( 'NONE', *, *, #9508, .F. ) ;
#541 = CARTESIAN_POINT ( 'NONE',  ( 0.000000000000000000, 0.000000000000000000, 1.000000000000000000 ) ) ;
#542 = DIRECTION ( 'NONE',  ( 1.000000000000000000, 0.000000000000000000, 0.000000000000000000 ) ) ;
#543 = CARTESIAN_POINT ( 'NONE',  ( -3.909826107002860596, 8.641065831729461522, 6.857782953271941950E-17 ) ) ;
#544 = LINE ( 'NONE', #3302, #6484 ) ;
#545 = VECTOR ( 'NONE', #8559, 1000.000000000000000 ) ;
#546 = EDGE_LOOP ( 'NONE', ( #8097, #7998 ) ) ;
#547 = DIRECTION ( 'NONE',  ( -1.000000000000000000, -0.000000000000000000, 0.000000000000000000 ) ) ;
#548 = ORIENTED_EDGE ( 'NONE', *, *, #8419, .F. ) ;
#549 = EDGE_CURVE ( 'NONE', #5532, #11993, #8278, .T. ) ;
#550 = CARTESIAN_POINT ( 'NONE',  ( 8.800885721068839374, 6.316044917328129671, 10.00000000000000000 ) ) ;
#551 = ORIENTED_EDGE ( 'NONE', *, *, #5552, .T. ) ;
#552 = FACE_OUTER_BOUND ( 'NONE', #933, .T. ) ;
#553 = AXIS2_PLACEMENT_3D ( 'NONE', #11181, #7367, #11111 ) ;
#554 = CARTESIAN_POINT ( 'NONE',  ( 0.000000000000000000, 0.000000000000000000, 0.000000000000000000 ) ) ;
#555 = AXIS2_PLACEMENT_3D ( 'NONE', #7557, #6758, #3777 ) ;
#556 = EDGE_CURVE ( 'NONE', #5532, #8486, #6878, .T. ) ;
#557 = LINE ( 'NONE', #4291, #10055 ) ;
#558 = CARTESIAN_POINT ( 'NONE',  ( 0.7062845326068618590, -10.79445016380499212, 10.00000000000000000 ) ) ;
#559 = CARTESIAN_POINT ( 'NONE',  ( -10.00000000000000000, 0.000000000000000000, 0.000000000000000000 ) ) ;
#560 = CARTESIAN_POINT ( 'NONE',  ( 7.972781652389871354, 11.51689705412852405, 3.747395293195558847E-16 ) ) ;
#561 = DIRECTION ( 'NONE',  ( 0.000000000000000000, 0.000000000000000000, -1.000000000000000000 ) ) ;
#562 = ORIENTED_EDGE ( 'NONE', *, *, #3448, .F. ) ;
#563 = DIRECTION ( 'NONE',  ( -1.000000000000000000, 0.000000000000000000, 0.000000000000000000 ) ) ;
#564 = ORIENTED_EDGE ( 'NONE', *, *, #3143, .T. ) ;
#565 = AXIS2_PLACEMENT_3D ( 'NONE', #9349, #4232, #9292 ) ;
#566 = CYLINDRICAL_SURFACE ( 'NONE', #2787, 9.599999999999997868 ) ;
#567 = CARTESIAN_POINT ( 'NONE',  ( 0.000000000000000000, 9.039786367038837867, 21.14796121233199599 ) ) ;
#568 =( NAMED_UNIT ( * ) PLANE_ANGLE_UNIT ( ) SI_UNIT ( $, .RADIAN. ) );
#569 = ORIENTED_EDGE ( 'NONE', *, *, #2522, .T. ) ;
#570 = CARTESIAN_POINT ( 'NONE',  ( 0.000000000000000000, 0.000000000000000000, 0.000000000000000000 ) ) ;
#571 = DIRECTION ( 'NONE',  ( 0.000000000000000000, 0.000000000000000000, 1.000000000000000000 ) ) ;
#572 = CARTESIAN_POINT ( 'NONE',  ( 1.499999999999999556, -23.05871956130116018, -9.128825345753256215 ) ) ;
#573 = VECTOR ( 'NONE', #3606, 1000.000000000000000 ) ;
#574 = CIRCLE ( 'NONE', #2139, 9.599999999999996092 ) ;
#575 = CARTESIAN_POINT ( 'NONE',  ( 2.798030692818294085, 8.692477993603722197, 6.857782953271941950E-17 ) ) ;
#576 = DIRECTION ( 'NONE',  ( 0.000000000000000000, 0.000000000000000000, -1.000000000000000000 ) ) ;
#577 = CIRCLE ( 'NONE', #7215, 24.80000000000000071 ) ;
#578 = CYLINDRICAL_SURFACE ( 'NONE', #1563, 22.99899999999999878 ) ;
#579 = ORIENTED_EDGE ( 'NONE', *, *, #12044, .T. ) ;
#580 = ORIENTED_EDGE ( 'NONE', *, *, #3066, .F. ) ;
#581 = ORIENTED_EDGE ( 'NONE', *, *, #7048, .T. ) ;
#582 = CARTESIAN_POINT ( 'NONE',  ( -14.24631147015002242, -5.364320868108786833, 10.00000000000000000 ) ) ;
#583 = AXIS2_PLACEMENT_3D ( 'NONE', #10430, #10546, #7858 ) ;
#584 = DIRECTION ( 'NONE',  ( 1.000000000000000000, 0.000000000000000000, 0.000000000000000000 ) ) ;
#585 = CARTESIAN_POINT ( 'NONE',  ( -4.158289900079266133, 7.437556212723415605, 3.747395293195558847E-16 ) ) ;
#586 = VECTOR ( 'NONE', #10792, 1000.000000000000000 ) ;
#587 = EDGE_CURVE ( 'NONE', #8746, #9071, #10601, .T. ) ;
#588 = DIRECTION ( 'NONE',  ( -1.000000000000000000, 0.000000000000000000, 0.000000000000000000 ) ) ;
#589 = AXIS2_PLACEMENT_3D ( 'NONE', #5331, #1593, #11683 ) ;
#590 = EDGE_CURVE ( 'NONE', #10713, #4077, #5327, .T. ) ;
#591 = AXIS2_PLACEMENT_3D ( 'NONE', #249, #11578, #11511 ) ;
#592 = DIRECTION ( 'NONE',  ( 0.000000000000000000, 0.000000000000000000, 1.000000000000000000 ) ) ;
#593 = ORIENTED_EDGE ( 'NONE', *, *, #3174, .F. ) ;
#594 = ORIENTED_EDGE ( 'NONE', *, *, #7522, .F. ) ;
#595 = CARTESIAN_POINT ( 'NONE',  ( -5.414455899168761022, -12.47541146649038879, 10.00000000000000000 ) ) ;
#596 = EDGE_CURVE ( 'NONE', #6304, #1233, #11190, .T. ) ;
#597 = ORIENTED_EDGE ( 'NONE', *, *, #549, .T. ) ;
#598 = CARTESIAN_POINT ( 'NONE',  ( 3.000000000000000888, -13.62355943574006645, -17.97274125076088680 ) ) ;
#599 = CARTESIAN_POINT ( 'NONE',  ( 0.000000000000000000, 0.000000000000000000, 0.000000000000000000 ) ) ;
#600 = CARTESIAN_POINT ( 'NONE',  ( 0.000000000000000000, -6.532525787311115550, 21.58580335785674365 ) ) ;
#601 = CIRCLE ( 'NONE', #7436, 9.599999999999997868 ) ;
#602 = AXIS2_PLACEMENT_3D ( 'NONE', #7128, #11848, #6169 ) ;
#603 = CYLINDRICAL_SURFACE ( 'NONE', #6413, 22.99899999999999878 ) ;
#604 = EDGE_LOOP ( 'NONE', ( #8602, #11394, #3338, #9831 ) ) ;
#605 = AXIS2_PLACEMENT_3D ( 'NONE', #6063, #1471, #11807 ) ;
#606 = DIRECTION ( 'NONE',  ( 1.000000000000000000, 0.000000000000000000, 0.000000000000000000 ) ) ;
#607 = CARTESIAN_POINT ( 'NONE',  ( 3.000000000000000888, -24.02068490260608868, -6.168200451486002045 ) ) ;
#608 = CARTESIAN_POINT ( 'NONE',  ( -7.708066421255707290, 5.920849505456867945, 6.857782953271941950E-17 ) ) ;
#609 = EDGE_CURVE ( 'NONE', #8357, #2308, #4475, .T. ) ;
#610 = DIRECTION ( 'NONE',  ( -1.000000000000000000, 0.000000000000000000, 0.000000000000000000 ) ) ;
#611 = AXIS2_PLACEMENT_3D ( 'NONE', #8367, #8434, #12090 ) ;
#612 = EDGE_LOOP ( 'NONE', ( #7954, #10758, #1154, #8872 ) ) ;
#613 = DIRECTION ( 'NONE',  ( -1.000000000000000000, 0.000000000000000000, 0.000000000000000000 ) ) ;
#614 = CIRCLE ( 'NONE', #3942, 9.599999999999996092 ) ;
#615 = ORIENTED_EDGE ( 'NONE', *, *, #11895, .F. ) ;
#616 = ORIENTED_EDGE ( 'NONE', *, *, #5832, .T. ) ;
#617 = CARTESIAN_POINT ( 'NONE',  ( 5.657123057053187409, 5.504982807385219168, 10.00000000000000000 ) ) ;
#618 = ORIENTED_EDGE ( 'NONE', *, *, #5367, .T. ) ;
#619 = EDGE_CURVE ( 'NONE', #6675, #1739, #4934, .T. ) ;
#620 = CARTESIAN_POINT ( 'NONE',  ( -10.00000000000000000, 0.000000000000000000, 0.000000000000000000 ) ) ;
#621 = FILL_AREA_STYLE ('',( #9865 ) ) ;
#622 = VERTEX_POINT ( 'NONE', #7936 ) ;
#623 = DIRECTION ( 'NONE',  ( -1.000000000000000000, -0.000000000000000000, 0.000000000000000000 ) ) ;
#624 = DIRECTION ( 'NONE',  ( 1.000000000000000000, -0.000000000000000000, -0.000000000000000000 ) ) ;
#625 = CARTESIAN_POINT ( 'NONE',  ( 7.252227276002106038, 5.017415995114419047, 10.00000000000000000 ) ) ;
#626 = EDGE_CURVE ( 'NONE', #8343, #518, #3071, .T. ) ;
#627 = DIRECTION ( 'NONE',  ( -1.000000000000000000, 0.000000000000000000, -0.000000000000000000 ) ) ;
#628 = CARTESIAN_POINT ( 'NONE',  ( -1.035167565893234443, -12.71157708251009133, 3.747395293195558847E-16 ) ) ;
#629 = CARTESIAN_POINT ( 'NONE',  ( 3.000000000000000888, 13.79477846460820700, -18.40266524480574972 ) ) ;
#630 = DIRECTION ( 'NONE',  ( -1.000000000000000000, -0.000000000000000000, -0.000000000000000000 ) ) ;
#631 = AXIS2_PLACEMENT_3D ( 'NONE', #10969, #3625, #3568 ) ;
#632 = EDGE_LOOP ( 'NONE', ( #7025, #6641, #7576, #734 ) ) ;
#633 = EDGE_CURVE ( 'NONE', #1751, #5065, #1965, .T. ) ;
#634 = LINE ( 'NONE', #10859, #8056 ) ;
#635 = DIRECTION ( 'NONE',  ( 0.000000000000000000, 0.000000000000000000, 1.000000000000000000 ) ) ;
#636 = EDGE_LOOP ( 'NONE', ( #11452, #11857, #7283, #1512 ) ) ;
#637 = CARTESIAN_POINT ( 'NONE',  ( 3.000000000000000888, 11.79560690673872259, 19.74380051311544193 ) ) ;
#638 = CARTESIAN_POINT ( 'NONE',  ( 0.000000000000000000, -5.135568396239877487, -21.96011696265496838 ) ) ;
#639 = LINE ( 'NONE', #9139, #6527 ) ;
#640 = CARTESIAN_POINT ( 'NONE',  ( 1.661435237661583297, -7.700870200009183542, 10.00000000000000000 ) ) ;
#641 = CARTESIAN_POINT ( 'NONE',  ( -4.625218816436122538, 8.325684435358754243, 6.857782953271941950E-17 ) ) ;
#642 = LINE ( 'NONE', #3336, #1232 ) ;
#643 = DIRECTION ( 'NONE',  ( -1.000000000000000000, -1.445602896647338917E-16, 0.000000000000000000 ) ) ;
#644 = AXIS2_PLACEMENT_3D ( 'NONE', #7358, #6569, #7420 ) ;
#645 = EDGE_LOOP ( 'NONE', ( #4129, #6737, #551, #9664 ) ) ;
#646 = ORIENTED_EDGE ( 'NONE', *, *, #6981, .F. ) ;
#647 = ADVANCED_FACE ( 'NONE', ( #2949 ), #10345, .T. ) ;
#648 = ORIENTED_EDGE ( 'NONE', *, *, #11063, .T. ) ;
#649 = AXIS2_PLACEMENT_3D ( 'NONE', #4290, #10847, #1716 ) ;
#650 = CARTESIAN_POINT ( 'NONE',  ( -2.069312577552833154, -12.54440658741724235, 10.00000000000000000 ) ) ;
#651 = AXIS2_PLACEMENT_3D ( 'NONE', #598, #6300, #8928 ) ;
#652 = DIRECTION ( 'NONE',  ( 0.000000000000000000, 0.000000000000000000, 1.000000000000000000 ) ) ;
#653 = CIRCLE ( 'NONE', #10623, 22.99899999999999878 ) ;
#654 = CARTESIAN_POINT ( 'NONE',  ( 0.03696586647634111239, -4.250492970015663730, 10.00000000000000000 ) ) ;
#655 = CARTESIAN_POINT ( 'NONE',  ( -4.158472309566738190, 3.840014155104740201, 3.747395293195558847E-16 ) ) ;
#656 = CIRCLE ( 'NONE', #2616, 9.599999999999997868 ) ;
#657 = CARTESIAN_POINT ( 'NONE',  ( 0.000000000000000000, -15.40502424595158359, 19.43515443678397503 ) ) ;
#658 = DIRECTION ( 'NONE',  ( -1.000000000000000000, 0.000000000000000000, 0.000000000000000000 ) ) ;
#659 = EDGE_LOOP ( 'NONE', ( #6044, #5887 ) ) ;
#660 = ORIENTED_EDGE ( 'NONE', *, *, #392, .F. ) ;
#661 = ITEM_DEFINED_TRANSFORMATION ( 'NONE', 'NONE', #2360,  #8474 ) ;
#662 = VERTEX_POINT ( 'NONE', #2144 ) ;
#663 = CARTESIAN_POINT ( 'NONE',  ( -1.784247137544766604, 5.123456263349899231, 10.00000000000000000 ) ) ;
#664 = DIRECTION ( 'NONE',  ( -1.000000000000000000, 0.000000000000000000, 0.000000000000000000 ) ) ;
#665 = CIRCLE ( 'NONE', #8686, 22.99900000000000233 ) ;
#666 = DIRECTION ( 'NONE',  ( -1.000000000000000000, 0.000000000000000000, 0.000000000000000000 ) ) ;
#667 = ORIENTED_EDGE ( 'NONE', *, *, #4953, .F. ) ;
#668 = FACE_OUTER_BOUND ( 'NONE', #4480, .T. ) ;
#669 = EDGE_CURVE ( 'NONE', #11061, #8500, #8522, .T. ) ;
#670 = DIRECTION ( 'NONE',  ( -1.000000000000000000, 0.000000000000000000, 0.000000000000000000 ) ) ;
#671 = CARTESIAN_POINT ( 'NONE',  ( 10.96671743108978525, -3.132869264233209439, 6.857782953271941950E-17 ) ) ;
#672 = DIRECTION ( 'NONE',  ( -1.000000000000000000, -0.000000000000000000, 0.000000000000000000 ) ) ;
#673 = AXIS2_PLACEMENT_3D ( 'NONE', #11695, #4235, #4054 ) ;
#674 = CARTESIAN_POINT ( 'NONE',  ( 3.000000000000000888, -2.811977935937933104, 22.37663021667342989 ) ) ;
#675 = ORIENTED_EDGE ( 'NONE', *, *, #143, .F. ) ;
#676 = ORIENTED_EDGE ( 'NONE', *, *, #5843, .F. ) ;
#677 = CARTESIAN_POINT ( 'NONE',  ( 7.536008357046525497, 0.2705779428718255719, 10.00000000000000000 ) ) ;
#678 = ADVANCED_FACE ( 'NONE', ( #5823 ), #3283, .T. ) ;
#679 = VERTEX_POINT ( 'NONE', #5641 ) ;
#680 = CARTESIAN_POINT ( 'NONE',  ( 0.000000000000000000, 3.623565124517105218, 24.53384959170458757 ) ) ;
#681 = ORIENTED_EDGE ( 'NONE', *, *, #9202, .T. ) ;
#682 = EDGE_CURVE ( 'NONE', #9917, #762, #11766, .T. ) ;
#683 = DIRECTION ( 'NONE',  ( 1.000000000000000000, 0.000000000000000000, 0.000000000000000000 ) ) ;
#684 = DIRECTION ( 'NONE',  ( 0.000000000000000000, 0.000000000000000000, 1.000000000000000000 ) ) ;
#685 = CARTESIAN_POINT ( 'NONE',  ( -0.2556890074706391625, -7.756263830888999067, 10.00000000000000000 ) ) ;
#686 = FACE_OUTER_BOUND ( 'NONE', #5474, .T. ) ;
#687 = DIRECTION ( 'NONE',  ( -1.000000000000000000, 0.000000000000000000, -0.000000000000000000 ) ) ;
#688 = ORIENTED_EDGE ( 'NONE', *, *, #6545, .T. ) ;
#689 = DIRECTION ( 'NONE',  ( 0.000000000000000000, 0.000000000000000000, -1.000000000000000000 ) ) ;
#690 = ORIENTED_EDGE ( 'NONE', *, *, #8658, .T. ) ;
#691 = CIRCLE ( 'NONE', #11447, 9.599999999999997868 ) ;
#692 = CARTESIAN_POINT ( 'NONE',  ( 6.411932913580776550, 4.469049885107575726, 3.747395293195558847E-16 ) ) ;
#693 = DIRECTION ( 'NONE',  ( -1.000000000000000000, -0.000000000000000000, -0.000000000000000000 ) ) ;
#694 = SURFACE_STYLE_USAGE ( .BOTH. , #4367 ) ;
#695 = ORIENTED_EDGE ( 'NONE', *, *, #11382, .T. ) ;
#696 = CARTESIAN_POINT ( 'NONE',  ( 3.000000000000000888, 14.74749645580034496, -17.06259499759930165 ) ) ;
#697 = DIRECTION ( 'NONE',  ( -1.000000000000000000, -0.000000000000000000, 0.000000000000000000 ) ) ;
#698 = CARTESIAN_POINT ( 'NONE',  ( -6.211147023100844322, 2.816369743025010308, 10.00000000000000000 ) ) ;
#699 = CARTESIAN_POINT ( 'NONE',  ( -8.665663522307772482, -5.581295667939712324, 6.857782953271941950E-17 ) ) ;
#700 = CARTESIAN_POINT ( 'NONE',  ( 0.000000000000000000, 5.117118920208487687, 22.42251312757881365 ) ) ;
#701 = CARTESIAN_POINT ( 'NONE',  ( 3.000000000000000888, -9.667200211209685534, -20.86861857134744014 ) ) ;
#702 = ORIENTED_EDGE ( 'NONE', *, *, #8462, .F. ) ;
#703 = ORIENTED_EDGE ( 'NONE', *, *, #7091, .F. ) ;
#704 = EDGE_LOOP ( 'NONE', ( #4877, #4210, #1502, #2089 ) ) ;
#705 = EDGE_CURVE ( 'NONE', #1245, #3019, #4343, .T. ) ;
#706 = CARTESIAN_POINT ( 'NONE',  ( -5.318373871714366707, 13.46535835423756566, 10.00000000000000000 ) ) ;
#707 = CARTESIAN_POINT ( 'NONE',  ( 3.000000000000000888, -20.86861857134728027, -9.667200211210033700 ) ) ;
#708 = DIRECTION ( 'NONE',  ( -1.000000000000000000, 0.000000000000000000, 0.000000000000000000 ) ) ;
#709 = EDGE_CURVE ( 'NONE', #4686, #9990, #8581, .T. ) ;
#710 = CARTESIAN_POINT ( 'NONE',  ( -0.4771094043438768861, 5.286185534804329400, 3.747395293195558847E-16 ) ) ;
#711 = DIRECTION ( 'NONE',  ( 0.000000000000000000, 0.000000000000000000, 1.000000000000000000 ) ) ;
#712 = VERTEX_POINT ( 'NONE', #11451 ) ;
#713 = VECTOR ( 'NONE', #3546, 1000.000000000000000 ) ;
#714 = DIRECTION ( 'NONE',  ( -1.000000000000000000, 0.000000000000000000, 0.000000000000000000 ) ) ;
#715 = EDGE_LOOP ( 'NONE', ( #1395, #7130, #2723, #8615 ) ) ;
#716 = ORIENTED_EDGE ( 'NONE', *, *, #455, .T. ) ;
#717 = ORIENTED_EDGE ( 'NONE', *, *, #10247, .F. ) ;
#718 = DIRECTION ( 'NONE',  ( -1.000000000000000000, 0.000000000000000000, 0.000000000000000000 ) ) ;
#719 = DIRECTION ( 'NONE',  ( -1.000000000000000000, -0.000000000000000000, -0.000000000000000000 ) ) ;
#720 = PRODUCT_DEFINITION_CONTEXT ( 'detailed design', #10992, 'design' ) ;
#721 = CARTESIAN_POINT ( 'NONE',  ( 3.000000000000000888, 10.87771529938162196, 19.75591328264889768 ) ) ;
#722 = DIRECTION ( 'NONE',  ( 1.000000000000000000, 0.000000000000000000, 0.000000000000000000 ) ) ;
#723 = DIRECTION ( 'NONE',  ( -1.000000000000000000, 0.000000000000000000, 0.000000000000000000 ) ) ;
#724 = CARTESIAN_POINT ( 'NONE',  ( 7.763517025772753044, -3.069710483245351451, 6.857782953271941950E-17 ) ) ;
#725 = CARTESIAN_POINT ( 'NONE',  ( 0.000000000000000000, -14.74749645579999857, -17.06259499759959297 ) ) ;
#726 = AXIS2_PLACEMENT_3D ( 'NONE', #5849, #9637, #2109 ) ;
#727 = CARTESIAN_POINT ( 'NONE',  ( 3.000000000000000888, 0.000000000000000000, 0.000000000000000000 ) ) ;
#728 = ORIENTED_EDGE ( 'NONE', *, *, #4002, .F. ) ;
#729 = AXIS2_PLACEMENT_3D ( 'NONE', #1436, #9880, #8848 ) ;
#730 = VERTEX_POINT ( 'NONE', #7530 ) ;
#731 = CARTESIAN_POINT ( 'NONE',  ( 6.723006375386864519, 3.907299473125435796, 10.00000000000000000 ) ) ;
#732 = ORIENTED_EDGE ( 'NONE', *, *, #5614, .F. ) ;
#733 = CARTESIAN_POINT ( 'NONE',  ( 3.000000000000000888, 17.06259499759944021, 14.74749645580017088 ) ) ;
#734 = ORIENTED_EDGE ( 'NONE', *, *, #1836, .T. ) ;
#735 = ADVANCED_FACE ( 'NONE', ( #8866 ), #469, .T. ) ;
#736 = CYLINDRICAL_SURFACE ( 'NONE', #9441, 9.599999999999997868 ) ;
#737 =( REPRESENTATION_RELATIONSHIP ('NONE','NONE', #8743, #842 ) REPRESENTATION_RELATIONSHIP_WITH_TRANSFORMATION ( #5378 )SHAPE_REPRESENTATION_RELATIONSHIP( ) );
#738 = DIRECTION ( 'NONE',  ( 0.000000000000000000, 0.000000000000000000, 1.000000000000000000 ) ) ;
#739 = CARTESIAN_POINT ( 'NONE',  ( 17.46093749967478104, -1.431715403549062460, 6.857782953271941950E-17 ) ) ;
#740 = CIRCLE ( 'NONE', #10111, 9.599999999999996092 ) ;
#741 = DIRECTION ( 'NONE',  ( 0.000000000000000000, 0.5877852522924690293, 0.8090169943749504489 ) ) ;
#742 = PRODUCT_RELATED_PRODUCT_CATEGORY ( 'part', '', ( #8642 ) ) ;
#743 = LINE ( 'NONE', #3570, #11739 ) ;
#744 = ORIENTED_EDGE ( 'NONE', *, *, #10443, .F. ) ;
#745 = DIRECTION ( 'NONE',  ( -1.000000000000000000, -0.000000000000000000, -0.000000000000000000 ) ) ;
#746 = ADVANCED_FACE ( 'NONE', ( #3811 ), #3925, .T. ) ;
#747 = ORIENTED_EDGE ( 'NONE', *, *, #11296, .F. ) ;
#748 = EDGE_CURVE ( 'NONE', #3296, #4404, #2888, .T. ) ;
#749 = CARTESIAN_POINT ( 'NONE',  ( 0.8073695008816142993, 5.181225205791315958, 3.747395293195558847E-16 ) ) ;
#750 = AXIS2_PLACEMENT_3D ( 'NONE', #910, #10269, #9233 ) ;
#751 = CARTESIAN_POINT ( 'NONE',  ( 0.000000000000000000, 8.753070780933430939, -20.78471918669851703 ) ) ;
#752 =( LENGTH_UNIT ( ) NAMED_UNIT ( * ) SI_UNIT ( .MILLI., .METRE. ) );
#753 = ORIENTED_EDGE ( 'NONE', *, *, #3793, .T. ) ;
#754 = DIRECTION ( 'NONE',  ( -1.000000000000000000, -0.000000000000000000, 0.000000000000000000 ) ) ;
#755 = DIRECTION ( 'NONE',  ( 1.000000000000000000, -0.000000000000000000, -0.000000000000000000 ) ) ;
#756 = CARTESIAN_POINT ( 'NONE',  ( 2.529667540517110513, -4.392173529266737653, 10.00000000000000000 ) ) ;
#757 = CARTESIAN_POINT ( 'NONE',  ( 4.138106518798946531, 8.052838533163340529, 6.857782953271941950E-17 ) ) ;
#758 = DIRECTION ( 'NONE',  ( 0.000000000000000000, 0.000000000000000000, 1.000000000000000000 ) ) ;
#759 = CIRCLE ( 'NONE', #7793, 22.99900000000000233 ) ;
#760 = CARTESIAN_POINT ( 'NONE',  ( 3.000000000000000888, 19.74380051311556628, -11.79560690673851475 ) ) ;
#761 = ORIENTED_EDGE ( 'NONE', *, *, #7434, .T. ) ;
#762 = VERTEX_POINT ( 'NONE', #5708 ) ;
#763 = CARTESIAN_POINT ( 'NONE',  ( -8.499083411061075566, 11.86528080735166490, 10.00000000000000000 ) ) ;
#764 = AXIS2_PLACEMENT_3D ( 'NONE', #9528, #11253, #7566 ) ;
#765 = CIRCLE ( 'NONE', #11129, 9.599999999999996092 ) ;
#766 = CYLINDRICAL_SURFACE ( 'NONE', #2507, 1.500000000000000222 ) ;
#767 = EDGE_CURVE ( 'NONE', #7710, #10871, #9435, .T. ) ;
#768 = DIRECTION ( 'NONE',  ( 0.000000000000000000, 0.000000000000000000, 1.000000000000000000 ) ) ;
#769 = CIRCLE ( 'NONE', #6825, 24.80000000000000071 ) ;
#770 = CARTESIAN_POINT ( 'NONE',  ( 1.831757423467612389, 7.960349185506225389, 3.747395293195558847E-16 ) ) ;
#771 = EDGE_CURVE ( 'NONE', #4202, #11830, #11175, .T. ) ;
#772 = LINE ( 'NONE', #3352, #10188 ) ;
#773 = ORIENTED_EDGE ( 'NONE', *, *, #5743, .F. ) ;
#774 = CARTESIAN_POINT ( 'NONE',  ( 3.000000000000000888, -5.135568396239877487, -21.96011696265496838 ) ) ;
#775 = ORIENTED_EDGE ( 'NONE', *, *, #5689, .F. ) ;
#776 = AXIS2_PLACEMENT_3D ( 'NONE', #9692, #4925, #7791 ) ;
#777 = ORIENTED_EDGE ( 'NONE', *, *, #11884, .F. ) ;
#778 = CARTESIAN_POINT ( 'NONE',  ( 3.000000000000000888, 17.71842311621530541, 17.35216073792446778 ) ) ;
#779 = CARTESIAN_POINT ( 'NONE',  ( 3.000000000000000888, 9.128825345753341480, -23.05871956130113176 ) ) ;
#780 = ADVANCED_FACE ( 'NONE', ( #10410 ), #2028, .T. ) ;
#781 = FACE_OUTER_BOUND ( 'NONE', #365, .T. ) ;
#782 = CIRCLE ( 'NONE', #7616, 9.599999999999997868 ) ;
#783 = DIRECTION ( 'NONE',  ( -0.000000000000000000, -0.000000000000000000, -1.000000000000000000 ) ) ;
#784 = CARTESIAN_POINT ( 'NONE',  ( 3.000000000000000888, -22.90635393027947941, 2.062268319295487817 ) ) ;
#785 = DIRECTION ( 'NONE',  ( 0.000000000000000000, 0.8090169943749486725, -0.5877852522924714718 ) ) ;
#786 = DIRECTION ( 'NONE',  ( 0.000000000000000000, 0.000000000000000000, -1.000000000000000000 ) ) ;
#787 = ORIENTED_EDGE ( 'NONE', *, *, #5743, .T. ) ;
#788 = ORIENTED_EDGE ( 'NONE', *, *, #8191, .F. ) ;
#789 = DIRECTION ( 'NONE',  ( -1.000000000000000000, 0.000000000000000000, 0.000000000000000000 ) ) ;
#790 = VECTOR ( 'NONE', #5279, 1000.000000000000000 ) ;
#791 = ORIENTED_EDGE ( 'NONE', *, *, #8074, .F. ) ;
#792 = ORIENTED_EDGE ( 'NONE', *, *, #8917, .F. ) ;
#793 = VECTOR ( 'NONE', #10087, 1000.000000000000000 ) ;
#794 = CARTESIAN_POINT ( 'NONE',  ( 7.195390336726611658, 2.736402267197346028, 10.00000000000000000 ) ) ;
#795 = VECTOR ( 'NONE', #10033, 1000.000000000000000 ) ;
#796 = CIRCLE ( 'NONE', #4317, 22.99900000000000233 ) ;
#797 = ORIENTED_EDGE ( 'NONE', *, *, #242, .T. ) ;
#798 = CARTESIAN_POINT ( 'NONE',  ( 3.000000000000000888, -6.779701584702886308, 21.97702544527755109 ) ) ;
#799 = STYLED_ITEM ( 'NONE', ( #10298 ), #8499 ) ;
#800 = ORIENTED_EDGE ( 'NONE', *, *, #8832, .F. ) ;
#801 = CARTESIAN_POINT ( 'NONE',  ( 3.000000000000000888, -11.79560690673858403, -19.74380051311552364 ) ) ;
#802 = FACE_OUTER_BOUND ( 'NONE', #2919, .T. ) ;
#803 = CARTESIAN_POINT ( 'NONE',  ( 3.017784444055084503, -16.62017357425735753, 6.857782953271941950E-17 ) ) ;
#804 = AXIS2_PLACEMENT_3D ( 'NONE', #10853, #7966, #443 ) ;
#805 = DIRECTION ( 'NONE',  ( -1.000000000000000000, 0.000000000000000000, 0.000000000000000000 ) ) ;
#806 = CIRCLE ( 'NONE', #2015, 9.599999999999997868 ) ;
#807 = AXIS2_PLACEMENT_3D ( 'NONE', #10687, #5057, #2244 ) ;
#808 = CYLINDRICAL_SURFACE ( 'NONE', #8433, 24.80000000000000071 ) ;
#809 = ORIENTED_EDGE ( 'NONE', *, *, #6284, .T. ) ;
#810 = ORIENTED_EDGE ( 'NONE', *, *, #4224, .T. ) ;
#811 = DIRECTION ( 'NONE',  ( 0.000000000000000000, 0.000000000000000000, 1.000000000000000000 ) ) ;
#812 = ORIENTED_EDGE ( 'NONE', *, *, #4126, .T. ) ;
#813 = CARTESIAN_POINT ( 'NONE',  ( 7.527773320476327079, 0.8933511214758176333, 3.747395293195558847E-16 ) ) ;
#814 = CLOSED_SHELL ( 'NONE', ( #10354, #9816, #7402, #7243, #7988, #5762, #1031, #7711, #7647, #5316, #9141, #9675 ) ) ;
#815 = FACE_OUTER_BOUND ( 'NONE', #4398, .T. ) ;
#816 = FILL_AREA_STYLE_COLOUR ( '', #8664 ) ;
#817 = AXIS2_PLACEMENT_3D ( 'NONE', #515, #10063, #9091 ) ;
#818 = CARTESIAN_POINT ( 'NONE',  ( 0.000000000000000000, 13.28910708463157420, -20.93895013827567553 ) ) ;
#819 = EDGE_CURVE ( 'NONE', #11808, #6397, #9010, .T. ) ;
#820 = DIRECTION ( 'NONE',  ( 1.000000000000000000, 0.000000000000000000, 0.000000000000000000 ) ) ;
#821 = FACE_OUTER_BOUND ( 'NONE', #6585, .T. ) ;
#823 = EDGE_CURVE ( 'NONE', #916, #8820, #10378, .T. ) ;
#822 = CARTESIAN_POINT ( 'NONE',  ( 2.529667540516381319, -4.392173529266732324, 6.857782953271941950E-17 ) ) ;
#824 = CARTESIAN_POINT ( 'NONE',  ( 3.000000000000000888, 0.000000000000000000, 0.000000000000000000 ) ) ;
#825 = EDGE_CURVE ( 'NONE', #4657, #6571, #6084, .T. ) ;
#826 = CIRCLE ( 'NONE', #5120, 9.599999999999997868 ) ;
#827 = DIRECTION ( 'NONE',  ( 0.000000000000000000, -0.8660254037844328234, -0.5000000000000101030 ) ) ;
#828 = CIRCLE ( 'NONE', #8846, 22.99899999999999523 ) ;
#829 = ORIENTED_EDGE ( 'NONE', *, *, #10768, .F. ) ;
#830 = ORIENTED_EDGE ( 'NONE', *, *, #1712, .T. ) ;
#831 = CARTESIAN_POINT ( 'NONE',  ( 19.99999999999999645, 2.449293598294706119E-15, 20.00000000000000000 ) ) ;
#832 = CARTESIAN_POINT ( 'NONE',  ( -10.00031051369627200, 6.213292778947749007, 10.00000000000000000 ) ) ;
#833 = EDGE_CURVE ( 'NONE', #7905, #2790, #10011, .T. ) ;
#834 = PRESENTATION_LAYER_ASSIGNMENT (  '', '', ( #6110 ) ) ;
#835 = CARTESIAN_POINT ( 'NONE',  ( 0.000000000000000000, 23.88662356770115380, 6.668524164681710609 ) ) ;
#836 = DIRECTION ( 'NONE',  ( -1.000000000000000000, 0.000000000000000000, 0.000000000000000000 ) ) ;
#837 = EDGE_CURVE ( 'NONE', #5148, #6438, #9793, .T. ) ;
#838 = CARTESIAN_POINT ( 'NONE',  ( -3.937910939466568117, -8.732312745279397603, 3.747395293195558847E-16 ) ) ;
#839 = DIRECTION ( 'NONE',  ( -1.000000000000000000, 0.000000000000000000, 0.000000000000000000 ) ) ;
#840 = FACE_OUTER_BOUND ( 'NONE', #7883, .T. ) ;
#841 = ORIENTED_EDGE ( 'NONE', *, *, #3703, .F. ) ;
#842 = SHAPE_REPRESENTATION ( 'spring holder_ISO - Spur gear 0.8M 60T 20PA 3FW ---S60A75H50L8.0N', ( #8474 ), #6316 ) ;
#843 = VERTEX_POINT ( 'NONE', #1693 ) ;
#844 = AXIS2_PLACEMENT_3D ( 'NONE', #3010, #8755, #300 ) ;
#845 = VERTEX_POINT ( 'NONE', #7187 ) ;
#846 = EDGE_CURVE ( 'NONE', #474, #5072, #8122, .T. ) ;
#847 = ORIENTED_EDGE ( 'NONE', *, *, #4792, .T. ) ;
#848 = FACE_OUTER_BOUND ( 'NONE', #10159, .T. ) ;
#849 = CARTESIAN_POINT ( 'NONE',  ( 3.000000000000000888, 19.10918332567957734, 15.80756504416697084 ) ) ;
#850 = CARTESIAN_POINT ( 'NONE',  ( 3.000000000000000888, -22.47229024614978599, 1.901833551798177036 ) ) ;
#851 = EDGE_CURVE ( 'NONE', #5379, #4686, #8435, .T. ) ;
#852 = UNCERTAINTY_MEASURE_WITH_UNIT (LENGTH_MEASURE( 1.000000000000000082E-05 ), #3873, 'distance_accuracy_value', 'NONE');
#853 = DIRECTION ( 'NONE',  ( 0.000000000000000000, 0.000000000000000000, -1.000000000000000000 ) ) ;
#854 = AXIS2_PLACEMENT_3D ( 'NONE', #4707, #8379, #12098 ) ;
#855 = CYLINDRICAL_SURFACE ( 'NONE', #10629, 22.99899999999999878 ) ;
#856 = CARTESIAN_POINT ( 'NONE',  ( -13.83044629298881034, 5.462350471645222250, 3.747395293195558847E-16 ) ) ;
#857 = CARTESIAN_POINT ( 'NONE',  ( 8.393308867179008814, -1.106660293010312213, 6.857782953271941950E-17 ) ) ;
#858 = CARTESIAN_POINT ( 'NONE',  ( 0.000000000000000000, 0.000000000000000000, 0.000000000000000000 ) ) ;
#859 = ORIENTED_EDGE ( 'NONE', *, *, #1247, .T. ) ;
#860 = ORIENTED_EDGE ( 'NONE', *, *, #3665, .T. ) ;
#861 = DIRECTION ( 'NONE',  ( 0.000000000000000000, 0.000000000000000000, 1.000000000000000000 ) ) ;
#862 = VERTEX_POINT ( 'NONE', #11792 ) ;
#863 = AXIS2_PLACEMENT_3D ( 'NONE', #11432, #2290, #6026 ) ;
#864 = ORIENTED_EDGE ( 'NONE', *, *, #8239, .F. ) ;
#865 = CARTESIAN_POINT ( 'NONE',  ( -3.432991321284830200, 4.402131891631372973, 10.00000000000000000 ) ) ;
#866 = EDGE_CURVE ( 'NONE', #12050, #1364, #7044, .T. ) ;
#867 = ORIENTED_EDGE ( 'NONE', *, *, #7879, .F. ) ;
#868 = DIRECTION ( 'NONE',  ( -1.000000000000000000, -0.000000000000000000, -0.000000000000000000 ) ) ;
#869 = ORIENTED_EDGE ( 'NONE', *, *, #875, .F. ) ;
#870 = CYLINDRICAL_SURFACE ( 'NONE', #2804, 11.50000000000000178 ) ;
#871 = CARTESIAN_POINT ( 'NONE',  ( 3.000000000000000888, 6.779701584703024864, -21.97702544527750845 ) ) ;
#872 = CARTESIAN_POINT ( 'NONE',  ( -5.542557460684662374, -4.854674288180239827, 10.00000000000000000 ) ) ;
#873 = CIRCLE ( 'NONE', #10645, 9.599999999999999645 ) ;
#874 = CARTESIAN_POINT ( 'NONE',  ( 0.000000000000000000, 19.29833442572359559, 11.67026512804553562 ) ) ;
#875 = EDGE_CURVE ( 'NONE', #9575, #2975, #1571, .T. ) ;
#876 = DIRECTION ( 'NONE',  ( 0.000000000000000000, 0.000000000000000000, 1.000000000000000000 ) ) ;
#877 = ORIENTED_EDGE ( 'NONE', *, *, #6147, .F. ) ;
#878 = DIRECTION ( 'NONE',  ( 0.000000000000000000, 0.000000000000000000, 1.000000000000000000 ) ) ;
#879 = ORIENTED_EDGE ( 'NONE', *, *, #1369, .T. ) ;
#880 = CARTESIAN_POINT ( 'NONE',  ( -0.7379871813790714885, -6.677365878963852808, 3.747395293195558847E-16 ) ) ;
#881 = VECTOR ( 'NONE', #10966, 1000.000000000000000 ) ;
#882 = CARTESIAN_POINT ( 'NONE',  ( 0.000000000000000000, 0.000000000000000000, 0.000000000000000000 ) ) ;
#883 = CARTESIAN_POINT ( 'NONE',  ( 0.000000000000000000, -13.72351598154883412, -20.65684170206505499 ) ) ;
#884 = DIRECTION ( 'NONE',  ( -1.000000000000000000, 0.000000000000000000, 0.000000000000000000 ) ) ;
#885 = CARTESIAN_POINT ( 'NONE',  ( 4.382127860174852785, -16.35473703246191235, 10.00000000000000000 ) ) ;
#886 = CARTESIAN_POINT ( 'NONE',  ( 0.3111040546027372677, -4.780743156735971944, 6.857782953271941950E-17 ) ) ;
#887 = DIRECTION ( 'NONE',  ( 0.000000000000000000, 0.000000000000000000, 1.000000000000000000 ) ) ;
#888 = CYLINDRICAL_SURFACE ( 'NONE', #5681, 9.599999999999997868 ) ;
#889 = ORIENTED_EDGE ( 'NONE', *, *, #4726, .F. ) ;
#890 = ORIENTED_EDGE ( 'NONE', *, *, #7426, .T. ) ;
#891 = DIRECTION ( 'NONE',  ( 0.000000000000000000, 0.000000000000000000, 1.000000000000000000 ) ) ;
#892 = CARTESIAN_POINT ( 'NONE',  ( 4.071483724746832067, 10.33449570568845211, 10.00000000000000000 ) ) ;
#893 = EDGE_CURVE ( 'NONE', #3541, #5364, #1781, .T. ) ;
#894 = FACE_OUTER_BOUND ( 'NONE', #9272, .T. ) ;
#895 = DIRECTION ( 'NONE',  ( -1.000000000000000000, 0.000000000000000000, -0.000000000000000000 ) ) ;
#896 = AXIS2_PLACEMENT_3D ( 'NONE', #8956, #11648, #6204 ) ;
#897 = CARTESIAN_POINT ( 'NONE',  ( 10.00611923916670953, -2.842981073525689517, 3.747395293195558847E-16 ) ) ;
#898 = LINE ( 'NONE', #3781, #9632 ) ;
#899 = DIRECTION ( 'NONE',  ( -1.000000000000000000, -0.000000000000000000, -0.000000000000000000 ) ) ;
#900 = VERTEX_POINT ( 'NONE', #657 ) ;
#901 = EDGE_CURVE ( 'NONE', #8749, #1851, #10773, .T. ) ;
#902 = ORIENTED_EDGE ( 'NONE', *, *, #11966, .T. ) ;
#903 = AXIS2_PLACEMENT_3D ( 'NONE', #9864, #10603, #1475 ) ;
#904 = EDGE_CURVE ( 'NONE', #12019, #9943, #4262, .T. ) ;
#905 = ORIENTED_EDGE ( 'NONE', *, *, #7737, .T. ) ;
#906 = CARTESIAN_POINT ( 'NONE',  ( 0.000000000000000000, 11.48910920600683738, 21.97817939804043874 ) ) ;
#907 = ADVANCED_FACE ( 'NONE', ( #6291 ), #9842, .T. ) ;
#908 = CARTESIAN_POINT ( 'NONE',  ( 0.000000000000000000, -22.15038895030651744, 4.240409074144028345 ) ) ;
#909 = FACE_OUTER_BOUND ( 'NONE', #10096, .T. ) ;
#910 = CARTESIAN_POINT ( 'NONE',  ( 17.49999999999999645, 0.000000000000000000, 6.857782953271941950E-17 ) ) ;
#911 = DIRECTION ( 'NONE',  ( 0.000000000000000000, 0.000000000000000000, 1.000000000000000000 ) ) ;
#912 = CIRCLE ( 'NONE', #11650, 22.99899999999999878 ) ;
#913 = CARTESIAN_POINT ( 'NONE',  ( -3.043536693350106681, 14.07442491708025756, 3.747395293195558847E-16 ) ) ;
#914 = CARTESIAN_POINT ( 'NONE',  ( -6.191802569540376666, -3.848120238389427072, 6.857782953271941950E-17 ) ) ;
#915 = DIRECTION ( 'NONE',  ( 0.000000000000000000, -0.2079116908177665313, 0.9781476007338041345 ) ) ;
#916 = VERTEX_POINT ( 'NONE', #8921 ) ;
#917 = ORIENTED_EDGE ( 'NONE', *, *, #10322, .F. ) ;
#918 = LINE ( 'NONE', #3732, #2567 ) ;
#919 = ORIENTED_EDGE ( 'NONE', *, *, #6762, .T. ) ;
#920 = ORIENTED_EDGE ( 'NONE', *, *, #8530, .T. ) ;
#921 = DIRECTION ( 'NONE',  ( 1.000000000000000000, -0.000000000000000000, -0.000000000000000000 ) ) ;
#922 = LINE ( 'NONE', #115, #11269 ) ;
#923 = ORIENTED_EDGE ( 'NONE', *, *, #3474, .T. ) ;
#924 = CARTESIAN_POINT ( 'NONE',  ( 3.000000000000000888, -17.31945870441136748, -15.13242714128137401 ) ) ;
#925 = CARTESIAN_POINT ( 'NONE',  ( 3.000000000000000888, 22.99643626497956816, 0.3433949777332492848 ) ) ;
#926 = CARTESIAN_POINT ( 'NONE',  ( -4.263796145714478847, -6.152586724582791433, 10.00000000000000000 ) ) ;
#927 = SURFACE_SIDE_STYLE ('',( #10231 ) ) ;
#928 = ADVANCED_FACE ( 'NONE', ( #1638 ), #7989, .T. ) ;
#929 = DIRECTION ( 'NONE',  ( 0.000000000000000000, 0.000000000000000000, 1.000000000000000000 ) ) ;
#930 = AXIS2_PLACEMENT_3D ( 'NONE', #696, #10058, #4429 ) ;
#931 = DIRECTION ( 'NONE',  ( 0.000000000000000000, 0.000000000000000000, 1.000000000000000000 ) ) ;
#932 = ORIENTED_EDGE ( 'NONE', *, *, #5174, .F. ) ;
#933 = EDGE_LOOP ( 'NONE', ( #6969, #1544, #1044, #3210 ) ) ;
#934 = DIRECTION ( 'NONE',  ( -1.000000000000000000, 0.000000000000000000, -0.000000000000000000 ) ) ;
#935 = ORIENTED_EDGE ( 'NONE', *, *, #4758, .F. ) ;
#936 = CARTESIAN_POINT ( 'NONE',  ( -4.158472309566738190, 3.840014155104740201, 3.747395293195558847E-16 ) ) ;
#937 = CARTESIAN_POINT ( 'NONE',  ( 0.000000000000000000, 0.000000000000000000, -5.000000000000000000 ) ) ;
#938 = EDGE_CURVE ( 'NONE', #3221, #10872, #2617, .T. ) ;
#939 = VECTOR ( 'NONE', #11932, 1000.000000000000000 ) ;
#940 = DIRECTION ( 'NONE',  ( 0.000000000000000000, -0.9781476007338079093, 0.2079116908177492118 ) ) ;
#941 = CARTESIAN_POINT ( 'NONE',  ( 0.000000000000000000, -24.75110766671651064, -1.556492618230893132 ) ) ;
#942 = CARTESIAN_POINT ( 'NONE',  ( 17.24531215409499296, -2.853661713830125013, 10.00000000000000000 ) ) ;
#943 = CARTESIAN_POINT ( 'NONE',  ( 5.893263639826756162, 6.717612500731040548, 6.857782953271941950E-17 ) ) ;
#944 = DIRECTION ( 'NONE',  ( -1.000000000000000000, 0.000000000000000000, 0.000000000000000000 ) ) ;
#945 = DIRECTION ( 'NONE',  ( -0.000000000000000000, -0.000000000000000000, -1.000000000000000000 ) ) ;
#946 = ORIENTED_EDGE ( 'NONE', *, *, #10281, .F. ) ;
#947 = ORIENTED_EDGE ( 'NONE', *, *, #9579, .T. ) ;
#948 = VECTOR ( 'NONE', #3473, 1000.000000000000000 ) ;
#949 = EDGE_LOOP ( 'NONE', ( #11530, #8082, #9226, #7103 ) ) ;
#950 = DIRECTION ( 'NONE',  ( -1.000000000000000000, -0.000000000000000000, -0.000000000000000000 ) ) ;
#951 = CARTESIAN_POINT ( 'NONE',  ( 10.39479819782869896, 2.258419626871297492, 10.00000000000000000 ) ) ;
#952 = CARTESIAN_POINT ( 'NONE',  ( 3.000000000000000888, 0.000000000000000000, 0.000000000000000000 ) ) ;
#953 = DIRECTION ( 'NONE',  ( -1.000000000000000000, -0.000000000000000000, -0.000000000000000000 ) ) ;
#954 = DIRECTION ( 'NONE',  ( 1.000000000000000000, -0.000000000000000000, -0.000000000000000000 ) ) ;
#955 = CARTESIAN_POINT ( 'NONE',  ( 1.454091968623351327, 11.13059540125182423, 3.747395293195558847E-16 ) ) ;
#956 = VECTOR ( 'NONE', #8634, 1000.000000000000000 ) ;
#957 = CIRCLE ( 'NONE', #12088, 9.599999999999997868 ) ;
#958 = DIRECTION ( 'NONE',  ( -1.000000000000000000, 0.000000000000000000, 0.000000000000000000 ) ) ;
#959 = DIRECTION ( 'NONE',  ( 0.000000000000000000, 0.000000000000000000, 1.000000000000000000 ) ) ;
#960 = ORIENTED_EDGE ( 'NONE', *, *, #11369, .T. ) ;
#961 = ORIENTED_EDGE ( 'NONE', *, *, #8693, .T. ) ;
#962 = VERTEX_POINT ( 'NONE', #4446 ) ;
#963 = CYLINDRICAL_SURFACE ( 'NONE', #7869, 22.99899999999999878 ) ;
#964 = CIRCLE ( 'NONE', #9169, 9.599999999999999645 ) ;
#965 = DIRECTION ( 'NONE',  ( 0.000000000000000000, 0.000000000000000000, -1.000000000000000000 ) ) ;
#966 = CARTESIAN_POINT ( 'NONE',  ( 0.000000000000000000, 0.000000000000000000, 0.000000000000000000 ) ) ;
#967 = FACE_BOUND ( 'NONE', #8620, .T. ) ;
#968 = DIRECTION ( 'NONE',  ( -1.000000000000000000, 0.000000000000000000, -0.000000000000000000 ) ) ;
#969 = EDGE_CURVE ( 'NONE', #10167, #9669, #6852, .T. ) ;
#970 = CARTESIAN_POINT ( 'NONE',  ( 10.36190401370965475, -8.216093097539266310, 3.747395293195558847E-16 ) ) ;
#971 = CARTESIAN_POINT ( 'NONE',  ( 1.022653496104248605, 6.171874473422422902, 6.857782953271941950E-17 ) ) ;
#972 = AXIS2_PLACEMENT_3D ( 'NONE', #7512, #3791, #8558 ) ;
#973 = EDGE_CURVE ( 'NONE', #6153, #9363, #772, .T. ) ;
#974 = AXIS2_PLACEMENT_3D ( 'NONE', #409, #2251, #3422 ) ;
#975 = DIRECTION ( 'NONE',  ( -1.000000000000000000, 0.000000000000000000, 0.000000000000000000 ) ) ;
#976 = DIRECTION ( 'NONE',  ( -1.000000000000000000, 0.000000000000000000, 0.000000000000000000 ) ) ;
#977 = ORIENTED_EDGE ( 'NONE', *, *, #8799, .T. ) ;
#978 = ORIENTED_EDGE ( 'NONE', *, *, #5853, .F. ) ;
#979 = CARTESIAN_POINT ( 'NONE',  ( 3.000000000000000888, -15.80756504416703656, 19.10918332567952760 ) ) ;
#980 = ORIENTED_EDGE ( 'NONE', *, *, #11817, .F. ) ;
#981 = ORIENTED_EDGE ( 'NONE', *, *, #6687, .F. ) ;
#982 = CYLINDRICAL_SURFACE ( 'NONE', #5934, 22.99899999999999878 ) ;
#983 = AXIS2_PLACEMENT_3D ( 'NONE', #8047, #5176, #8111 ) ;
#984 = DIRECTION ( 'NONE',  ( 0.000000000000000000, 0.9781476007338062439, -0.2079116908177564282 ) ) ;
#985 = ORIENTED_EDGE ( 'NONE', *, *, #2427, .T. ) ;
#986 = ADVANCED_FACE ( 'NONE', ( #10821 ), #2430, .T. ) ;
#987 = DIRECTION ( 'NONE',  ( -8.673617379884035472E-16, -1.000000000000000000, 0.000000000000000000 ) ) ;
#988 = FACE_OUTER_BOUND ( 'NONE', #10135, .T. ) ;
#989 = CARTESIAN_POINT ( 'NONE',  ( 17.24531215409252383, -2.853661713830123237, 6.857782953271941950E-17 ) ) ;
#990 = CARTESIAN_POINT ( 'NONE',  ( 0.0002901587068754535662, -4.749354241797641762, 5.000000000000000000 ) ) ;
#991 = CARTESIAN_POINT ( 'NONE',  ( -10.00000000000000000, 0.000000000000000000, 0.000000000000000000 ) ) ;
#992 = VERTEX_POINT ( 'NONE', #8059 ) ;
#993 = CIRCLE ( 'NONE', #10561, 19.99999999999999645 ) ;
#994 = VERTEX_POINT ( 'NONE', #10262 ) ;
#995 = DIRECTION ( 'NONE',  ( 0.000000000000000000, 0.000000000000000000, 1.000000000000000000 ) ) ;
#996 = AXIS2_PLACEMENT_3D ( 'NONE', #9018, #2467, #4298 ) ;
#997 = ORIENTED_EDGE ( 'NONE', *, *, #4678, .F. ) ;
#998 = EDGE_CURVE ( 'NONE', #11794, #6550, #10968, .T. ) ;
#999 = CARTESIAN_POINT ( 'NONE',  ( 4.163410377374356486, -12.26152398776834396, 10.00000000000000000 ) ) ;
#1000 = FACE_OUTER_BOUND ( 'NONE', #6266, .T. ) ;
#1001 =( LENGTH_UNIT ( ) NAMED_UNIT ( * ) SI_UNIT ( .MILLI., .METRE. ) );
#1002 = VECTOR ( 'NONE', #4734, 1000.000000000000000 ) ;
#1003 = EDGE_CURVE ( 'NONE', #9081, #662, #11301, .T. ) ;
#1005 = CIRCLE ( 'NONE', #7838, 9.599999999999997868 ) ;
#1004 = CARTESIAN_POINT ( 'NONE',  ( 3.000000000000000888, -11.79560690673858403, -19.74380051311552364 ) ) ;
#1006 = CIRCLE ( 'NONE', #5301, 22.99900000000000233 ) ;
#1007 = CYLINDRICAL_SURFACE ( 'NONE', #11040, 24.80000000000000071 ) ;
#1008 = CARTESIAN_POINT ( 'NONE',  ( -6.864300873105356082, 13.92024697337932082, 10.00000000000000000 ) ) ;
#1009 = CARTESIAN_POINT ( 'NONE',  ( -6.211147023100837217, 2.816369743025007644, 6.857782953271941950E-17 ) ) ;
#1010 = DIRECTION ( 'NONE',  ( 0.000000000000000000, 0.5000000000000011102, -0.8660254037844381525 ) ) ;
#1011 = DIRECTION ( 'NONE',  ( 0.000000000000000000, 0.000000000000000000, 1.000000000000000000 ) ) ;
#1012 = DIRECTION ( 'NONE',  ( 0.000000000000000000, 0.4067366430757948237, 0.9135454576426034201 ) ) ;
#1013 = VERTEX_POINT ( 'NONE', #10377 ) ;
#1014 = ADVANCED_FACE ( 'NONE', ( #840 ), #8307, .T. ) ;
#1015 = DIRECTION ( 'NONE',  ( 0.000000000000000000, 0.000000000000000000, 1.000000000000000000 ) ) ;
#1016 = CLOSED_SHELL ( 'NONE', ( #10067, #9974, #10631, #10029, #1210, #9209, #4991, #9798, #10209, #9430, #5118, #1787, #6730, #10852, #7083 ) ) ;
#1017 = VECTOR ( 'NONE', #3468, 1000.000000000000000 ) ;
#1018 = AXIS2_PLACEMENT_3D ( 'NONE', #3797, #10330, #10625 ) ;
#1019 = ORIENTED_EDGE ( 'NONE', *, *, #938, .T. ) ;
#1020 = CARTESIAN_POINT ( 'NONE',  ( 0.000000000000000000, 0.000000000000000000, 0.000000000000000000 ) ) ;
#1021 = CARTESIAN_POINT ( 'NONE',  ( -10.51222845931418703, 5.388985543801221745, 10.00000000000000000 ) ) ;
#1022 = DIRECTION ( 'NONE',  ( -1.000000000000000000, 0.000000000000000000, -0.000000000000000000 ) ) ;
#1023 = AXIS2_PLACEMENT_3D ( 'NONE', #1782, #9182, #1666 ) ;
#1024 = CARTESIAN_POINT ( 'NONE',  ( -6.925491926711623059, 5.292860106065907289, 3.747395293195558847E-16 ) ) ;
#1025 = AXIS2_PLACEMENT_3D ( 'NONE', #7648, #7528, #5820 ) ;
#1026 = AXIS2_PLACEMENT_3D ( 'NONE', #1109, #4841, #5145 ) ;
#1027 = CARTESIAN_POINT ( 'NONE',  ( 0.000000000000000000, 0.000000000000000000, 3.000000000000000000 ) ) ;
#1028 = DIRECTION ( 'NONE',  ( 0.000000000000000000, 0.000000000000000000, 1.000000000000000000 ) ) ;
#1029 = ORIENTED_EDGE ( 'NONE', *, *, #8017, .F. ) ;
#1030 = EDGE_CURVE ( 'NONE', #5818, #5746, #4634, .T. ) ;
#1031 = ADVANCED_FACE ( 'NONE', ( #3715, #5556 ), #2860, .F. ) ;
#1032 = ORIENTED_EDGE ( 'NONE', *, *, #5642, .T. ) ;
#1033 = ORIENTED_EDGE ( 'NONE', *, *, #3594, .T. ) ;
#1034 = CARTESIAN_POINT ( 'NONE',  ( 0.000000000000000000, 0.000000000000000000, 0.000000000000000000 ) ) ;
#1035 = VECTOR ( 'NONE', #9113, 1000.000000000000000 ) ;
#1036 = CARTESIAN_POINT ( 'NONE',  ( 0.000000000000000000, 0.000000000000000000, 0.000000000000000000 ) ) ;
#1037 = DIRECTION ( 'NONE',  ( 0.000000000000000000, 0.000000000000000000, -1.000000000000000000 ) ) ;
#1038 = CYLINDRICAL_SURFACE ( 'NONE', #7585, 22.99899999999999878 ) ;
#1039 = DIRECTION ( 'NONE',  ( -1.000000000000000000, -0.000000000000000000, -0.000000000000000000 ) ) ;
#1040 = CARTESIAN_POINT ( 'NONE',  ( -8.499083411061073789, 11.86528080735276269, 3.747395293195558847E-16 ) ) ;
#1041 = CIRCLE ( 'NONE', #3776, 5.000000000000000000 ) ;
#1042 = PLANE ( 'NONE',  #11528 ) ;
#1043 = EDGE_LOOP ( 'NONE', ( #5356, #3147, #11496, #8649 ) ) ;
#1044 = ORIENTED_EDGE ( 'NONE', *, *, #11340, .T. ) ;
#1045 = CARTESIAN_POINT ( 'NONE',  ( -1.103316172498668202, -16.73802372459124754, 10.00000000000000000 ) ) ;
#1046 = ORIENTED_EDGE ( 'NONE', *, *, #8832, .T. ) ;
#1047 = DIRECTION ( 'NONE',  ( -1.000000000000000000, -1.445602896647339163E-16, 0.000000000000000000 ) ) ;
#1048 = DIRECTION ( 'NONE',  ( 1.000000000000000000, 0.000000000000000000, -0.000000000000000000 ) ) ;
#1049 = VERTEX_POINT ( 'NONE', #11186 ) ;
#1050 = EDGE_CURVE ( 'NONE', #1721, #9359, #9285, .T. ) ;
#1051 = CARTESIAN_POINT ( 'NONE',  ( 3.000000000000000888, -11.79560690673886292, 19.74380051311536022 ) ) ;
#1052 = DIRECTION ( 'NONE',  ( -1.000000000000000000, 0.000000000000000000, -0.000000000000000000 ) ) ;
#1053 = CARTESIAN_POINT ( 'NONE',  ( 4.479449988082533807, -13.21383449271837840, 6.857782953271941950E-17 ) ) ;
#1054 = EDGE_CURVE ( 'NONE', #1140, #308, #5697, .T. ) ;
#1055 = CARTESIAN_POINT ( 'NONE',  ( 3.000000000000000888, 0.4575788569251889593, 22.54798042742718067 ) ) ;
#1056 = DIRECTION ( 'NONE',  ( -1.000000000000000000, -0.000000000000000000, -0.000000000000000000 ) ) ;
#1057 = AXIS2_PLACEMENT_3D ( 'NONE', #10270, #1887, #8448 ) ;
#1058 = ORIENTED_EDGE ( 'NONE', *, *, #1054, .T. ) ;
#1059 = CARTESIAN_POINT ( 'NONE',  ( 3.000000000000000888, -22.54798042742717357, 9.142421143074578538 ) ) ;
#1060 = ORIENTED_EDGE ( 'NONE', *, *, #3456, .F. ) ;
#1061 = EDGE_CURVE ( 'NONE', #1959, #9571, #11360, .T. ) ;
#1062 = CARTESIAN_POINT ( 'NONE',  ( -6.423942855642368777, 13.01866063961585951, 10.00000000000000000 ) ) ;
#1063 = EDGE_CURVE ( 'NONE', #264, #11972, #2764, .T. ) ;
#1064 = DIRECTION ( 'NONE',  ( 1.000000000000000000, 0.000000000000000000, 0.000000000000000000 ) ) ;
#1065 =( LENGTH_UNIT ( ) NAMED_UNIT ( * ) SI_UNIT ( .MILLI., .METRE. ) );
#1066 = AXIS2_PLACEMENT_3D ( 'NONE', #10300, #6685, #3028 ) ;
#1067 = CARTESIAN_POINT ( 'NONE',  ( 3.000000000000000888, 0.000000000000000000, 0.000000000000000000 ) ) ;
#1068 = CARTESIAN_POINT ( 'NONE',  ( 0.000000000000000000, 15.42759117534407309, -16.45023496161649845 ) ) ;
#1069 = CARTESIAN_POINT ( 'NONE',  ( -4.384918567263696332, -12.91535881965571342, 10.00000000000000000 ) ) ;
#1070 = DIRECTION ( 'NONE',  ( -1.000000000000000000, 0.000000000000000000, 0.000000000000000000 ) ) ;
#1071 = CARTESIAN_POINT ( 'NONE',  ( 0.000000000000000000, 0.000000000000000000, 0.000000000000000000 ) ) ;
#1072 = ORIENTED_EDGE ( 'NONE', *, *, #7174, .T. ) ;
#1073 = DIRECTION ( 'NONE',  ( 0.000000000000000000, 0.000000000000000000, 1.000000000000000000 ) ) ;
#1074 = VECTOR ( 'NONE', #6072, 1000.000000000000000 ) ;
#1075 = ORIENTED_EDGE ( 'NONE', *, *, #7340, .F. ) ;
#1076 = DIRECTION ( 'NONE',  ( -1.000000000000000000, 0.000000000000000000, -0.000000000000000000 ) ) ;
#1077 = CARTESIAN_POINT ( 'NONE',  ( 10.41236255589547177, -1.188820951657899361, 10.00000000000000000 ) ) ;
#1078 = CARTESIAN_POINT ( 'NONE',  ( 0.000000000000000000, 0.000000000000000000, 0.000000000000000000 ) ) ;
#1079 = CARTESIAN_POINT ( 'NONE',  ( -8.409270314015810044, 2.833341551407462244, 3.747395293195558847E-16 ) ) ;
#1080 = CARTESIAN_POINT ( 'NONE',  ( -14.19814495527598730, 7.008511237308412412, 6.857782953271941950E-17 ) ) ;
#1081 = CARTESIAN_POINT ( 'NONE',  ( 3.000000000000000888, 13.28910708463157775, -20.93895013827567908 ) ) ;
#1082 = VERTEX_POINT ( 'NONE', #2736 ) ;
#1083 = ADVANCED_FACE ( 'NONE', ( #1998 ), #6464, .T. ) ;
#1084 = VERTEX_POINT ( 'NONE', #6638 ) ;
#1085 = ORIENTED_EDGE ( 'NONE', *, *, #6750, .T. ) ;
#1086 = CARTESIAN_POINT ( 'NONE',  ( 0.000000000000000000, 1.901833551798570721, -22.47229024614975401 ) ) ;
#1087 = AXIS2_PLACEMENT_3D ( 'NONE', #11829, #1792, #10912 ) ;
#1088 = FACE_OUTER_BOUND ( 'NONE', #9309, .T. ) ;
#1089 = ORIENTED_EDGE ( 'NONE', *, *, #3366, .T. ) ;
#1090 = DIRECTION ( 'NONE',  ( 0.000000000000000000, 0.000000000000000000, 1.000000000000000000 ) ) ;
#1091 = CYLINDRICAL_SURFACE ( 'NONE', #11684, 9.599999999999997868 ) ;
#1092 = EDGE_CURVE ( 'NONE', #8486, #2895, #9605, .T. ) ;
#1093 = DIRECTION ( 'NONE',  ( -1.000000000000000000, -0.000000000000000000, 0.000000000000000000 ) ) ;
#1094 = CARTESIAN_POINT ( 'NONE',  ( -5.318373871714365819, 13.46535835423756389, 3.747395293195558847E-16 ) ) ;
#1095 = AXIS2_PLACEMENT_3D ( 'NONE', #2095, #5833, #9563 ) ;
#1096 = CARTESIAN_POINT ( 'NONE',  ( 0.000000000000000000, -20.78471918669854901, -8.753070780933368766 ) ) ;
#1097 = ORIENTED_EDGE ( 'NONE', *, *, #8084, .F. ) ;
#1098 = VERTEX_POINT ( 'NONE', #9466 ) ;
#1099 = DIRECTION ( 'NONE',  ( 1.000000000000000000, 0.000000000000000000, 0.000000000000000000 ) ) ;
#1100 = CARTESIAN_POINT ( 'NONE',  ( 0.000000000000000000, 1.901833551798254973, 22.47229024614977888 ) ) ;
#1101 = VERTEX_POINT ( 'NONE', #1081 ) ;
#1102 = LINE ( 'NONE', #169, #5352 ) ;
#1103 = CARTESIAN_POINT ( 'NONE',  ( 0.000000000000000000, 20.93895013827581408, 13.28910708463135215 ) ) ;
#1104 = ORIENTED_EDGE ( 'NONE', *, *, #7024, .T. ) ;
#1105 = CARTESIAN_POINT ( 'NONE',  ( 0.000000000000000000, 0.000000000000000000, 0.000000000000000000 ) ) ;
#1106 = CARTESIAN_POINT ( 'NONE',  ( 3.000000000000000888, 13.23915371906955052, 18.80635025205174671 ) ) ;
#1107 = CARTESIAN_POINT ( 'NONE',  ( -9.546882484473291797, 8.373557015400844961, 6.857782953271941950E-17 ) ) ;
#1108 = CARTESIAN_POINT ( 'NONE',  ( 50.00005079999999680, 0.000000000000000000, 4.000000000000000000 ) ) ;
#1109 = CARTESIAN_POINT ( 'NONE',  ( -10.00000000000000000, 0.000000000000000000, 0.000000000000000000 ) ) ;
#1110 = ORIENTED_EDGE ( 'NONE', *, *, #8556, .F. ) ;
#1111 = ORIENTED_EDGE ( 'NONE', *, *, #709, .T. ) ;
#1112 = CYLINDRICAL_SURFACE ( 'NONE', #203, 9.599999999999997868 ) ;
#1113 = EDGE_LOOP ( 'NONE', ( #6486, #11813, #10521, #6467 ) ) ;
#1114 = CARTESIAN_POINT ( 'NONE',  ( 11.62709622633371076, -6.461356448465072511, 10.00000000000000000 ) ) ;
#1115 = EDGE_CURVE ( 'NONE', #11364, #9575, #1005, .T. ) ;
#1116 = DIRECTION ( 'NONE',  ( 0.000000000000000000, 0.8660254037844398178, -0.4999999999999979461 ) ) ;
#1117 = FILL_AREA_STYLE ('',( #2038 ) ) ;
#1118 = DIRECTION ( 'NONE',  ( 0.000000000000000000, 0.2079116908177597312, -0.9781476007338056888 ) ) ;
#1119 = CARTESIAN_POINT ( 'NONE',  ( 3.000000000000000888, 5.135568396240338451, -21.96011696265485824 ) ) ;
#1120 = DIRECTION ( 'NONE',  ( -1.000000000000000000, 0.000000000000000000, 0.000000000000000000 ) ) ;
#1121 = CARTESIAN_POINT ( 'NONE',  ( -6.266017822847497420, 10.86399168115691438, 10.00000000000000000 ) ) ;
#1122 = CARTESIAN_POINT ( 'NONE',  ( 3.000000000000000888, 0.000000000000000000, 0.000000000000000000 ) ) ;
#1123 = CARTESIAN_POINT ( 'NONE',  ( -14.24631147015001886, -5.364320868109360596, 3.747395293195558847E-16 ) ) ;
#1124 = EDGE_CURVE ( 'NONE', #9845, #5068, #6583, .T. ) ;
#1125 = DIRECTION ( 'NONE',  ( 0.000000000000000000, 0.000000000000000000, 1.000000000000000000 ) ) ;
#1126 = ORIENTED_EDGE ( 'NONE', *, *, #3442, .F. ) ;
#1127 = EDGE_CURVE ( 'NONE', #11577, #2393, #10315, .T. ) ;
#1128 = CARTESIAN_POINT ( 'NONE',  ( 3.000000000000000888, -20.93895013827591001, 13.28910708463121360 ) ) ;
#1129 = ORIENTED_EDGE ( 'NONE', *, *, #6007, .F. ) ;
#1130 = ORIENTED_EDGE ( 'NONE', *, *, #4758, .T. ) ;
#1131 = AXIS2_PLACEMENT_3D ( 'NONE', #3999, #2397, #7847 ) ;
#1132 = DIRECTION ( 'NONE',  ( 0.000000000000000000, 0.000000000000000000, 1.000000000000000000 ) ) ;
#1133 = CARTESIAN_POINT ( 'NONE',  ( 7.402789038520873000, -0.9464297003978345835, 10.00000000000000000 ) ) ;
#1134 = CARTESIAN_POINT ( 'NONE',  ( -10.00000000000000000, 0.000000000000000000, 0.000000000000000000 ) ) ;
#1135 = CARTESIAN_POINT ( 'NONE',  ( -9.977213461302319786, -1.645879626164742593, 10.00000000000000000 ) ) ;
#1136 = ADVANCED_FACE ( 'NONE', ( #2672 ), #94, .T. ) ;
#1137 = CARTESIAN_POINT ( 'NONE',  ( -4.384918567263694555, -12.91535881965570631, 6.857782953271941950E-17 ) ) ;
#1138 = APPLICATION_CONTEXT ( 'automotive_design' ) ;
#1139 = CARTESIAN_POINT ( 'NONE',  ( 0.000000000000000000, 15.64281154287620446, -16.85990652506883691 ) ) ;
#1140 = VERTEX_POINT ( 'NONE', #4759 ) ;
#1141 = ORIENTED_EDGE ( 'NONE', *, *, #3972, .F. ) ;
#1142 = CARTESIAN_POINT ( 'NONE',  ( 3.000000000000000888, 0.000000000000000000, 0.000000000000000000 ) ) ;
#1143 = EDGE_CURVE ( 'NONE', #2754, #8927, #149, .T. ) ;
#1144 = DIRECTION ( 'NONE',  ( 1.000000000000000000, 0.000000000000000000, 0.000000000000000000 ) ) ;
#1145 = VERTEX_POINT ( 'NONE', #6937 ) ;
#1146 = VECTOR ( 'NONE', #1635, 1000.000000000000000 ) ;
#1147 = DIRECTION ( 'NONE',  ( 0.000000000000000000, 0.000000000000000000, 1.000000000000000000 ) ) ;
#1148 = DIRECTION ( 'NONE',  ( 0.000000000000000000, 0.000000000000000000, -1.000000000000000000 ) ) ;
#1149 = EDGE_CURVE ( 'NONE', #7092, #11368, #11944, .T. ) ;
#1150 = CARTESIAN_POINT ( 'NONE',  ( 3.000000000000000888, -22.83456483164690809, 2.745295967525920311 ) ) ;
#1151 = CARTESIAN_POINT ( 'NONE',  ( -9.045553118584754415, -8.482981269326389295, 3.747395293195558847E-16 ) ) ;
#1152 = CARTESIAN_POINT ( 'NONE',  ( 0.000000000000000000, -7.402892494506437160, 21.30300407174360444 ) ) ;
#1153 = AXIS2_PLACEMENT_3D ( 'NONE', #8000, #950, #10759 ) ;
#1154 = ORIENTED_EDGE ( 'NONE', *, *, #3077, .F. ) ;
#1155 = ORIENTED_EDGE ( 'NONE', *, *, #9457, .T. ) ;
#1156 = CARTESIAN_POINT ( 'NONE',  ( -14.19814495527487352, 7.008511237308415964, 10.00000000000000000 ) ) ;
#1157 = EDGE_CURVE ( 'NONE', #505, #6372, #11914, .T. ) ;
#1158 = ORIENTED_EDGE ( 'NONE', *, *, #8658, .F. ) ;
#1159 = CARTESIAN_POINT ( 'NONE',  ( 0.000000000000000000, -4.445336973061012387, 22.56530478845647636 ) ) ;
#1160 = CARTESIAN_POINT ( 'NONE',  ( 3.000000000000000888, -21.76479567747246691, 7.432877647175128999 ) ) ;
#1161 = DIRECTION ( 'NONE',  ( -1.000000000000000000, 0.000000000000000000, 0.000000000000000000 ) ) ;
#1162 = ORIENTED_EDGE ( 'NONE', *, *, #7713, .T. ) ;
#1163 = DIRECTION ( 'NONE',  ( 1.000000000000000000, 0.000000000000000000, -0.000000000000000000 ) ) ;
#1164 = DIRECTION ( 'NONE',  ( -1.000000000000000000, 0.000000000000000000, -0.000000000000000000 ) ) ;
#1165 = CARTESIAN_POINT ( 'NONE',  ( 2.259453438922057522, -13.68937604509904027, 6.857782953271941950E-17 ) ) ;
#1166 = CARTESIAN_POINT ( 'NONE',  ( 0.000000000000000000, 0.000000000000000000, 3.000000000000000000 ) ) ;
#1167 = VERTEX_POINT ( 'NONE', #10498 ) ;
#1168 = EDGE_CURVE ( 'NONE', #7859, #6466, #3553, .T. ) ;
#1169 = CARTESIAN_POINT ( 'NONE',  ( 0.000000000000000000, 0.000000000000000000, 0.000000000000000000 ) ) ;
#1170 = VERTEX_POINT ( 'NONE', #5918 ) ;
#1171 = LINE ( 'NONE', #2090, #4306 ) ;
#1172 = ORIENTED_EDGE ( 'NONE', *, *, #9523, .T. ) ;
#1173 = CARTESIAN_POINT ( 'NONE',  ( 13.24268851590354146, -2.403973981685017414, 10.00000000000000000 ) ) ;
#1174 = CARTESIAN_POINT ( 'NONE',  ( 0.000000000000000000, 0.000000000000000000, 0.000000000000000000 ) ) ;
#1175 = SHAPE_REPRESENTATION_RELATIONSHIP ( 'NONE' , 'NONE' ,  #6315, #8499 ) ;
#1176 = CARTESIAN_POINT ( 'NONE',  ( 1.500000000000000444, 20.65684170206491999, 13.72351598154904195 ) ) ;
#1177 = CARTESIAN_POINT ( 'NONE',  ( 3.000000000000000888, 0.000000000000000000, 0.000000000000000000 ) ) ;
#1178 = CARTESIAN_POINT ( 'NONE',  ( 9.056240860197965148, 7.682302481599247557, 10.00000000000000000 ) ) ;
#1179 = AXIS2_PLACEMENT_3D ( 'NONE', #3701, #8417, #7546 ) ;
#1180 = CARTESIAN_POINT ( 'NONE',  ( 0.000000000000000000, 0.000000000000000000, 0.000000000000000000 ) ) ;
#1181 = CARTESIAN_POINT ( 'NONE',  ( 6.600721363681633314, -14.58171973507987396, 3.747395293195558847E-16 ) ) ;
#1182 = CIRCLE ( 'NONE', #7240, 9.599999999999997868 ) ;
#1183 = CARTESIAN_POINT ( 'NONE',  ( 0.000000000000000000, -1.901833551798098876, -22.47229024614979309 ) ) ;
#1184 = ORIENTED_EDGE ( 'NONE', *, *, #11809, .F. ) ;
#1185 = AXIS2_PLACEMENT_3D ( 'NONE', #232, #2255, #6899 ) ;
#1186 = DIRECTION ( 'NONE',  ( -1.000000000000000000, -0.000000000000000000, -0.000000000000000000 ) ) ;
#1187 = ORIENTED_EDGE ( 'NONE', *, *, #8155, .T. ) ;
#1188 = ORIENTED_EDGE ( 'NONE', *, *, #2810, .F. ) ;
#1189 = CIRCLE ( 'NONE', #5695, 24.80000000000000071 ) ;
#1190 = PLANE ( 'NONE',  #7958 ) ;
#1191 = CARTESIAN_POINT ( 'NONE',  ( -4.428608208598376450, -4.627450663479480752, 10.00000000000000000 ) ) ;
#1192 = ADVANCED_FACE ( 'NONE', ( #395 ), #7805, .T. ) ;
#1193 = AXIS2_PLACEMENT_3D ( 'NONE', #9116, #12108, #861 ) ;
#1194 = DIRECTION ( 'NONE',  ( 1.000000000000000000, -0.000000000000000000, -0.000000000000000000 ) ) ;
#1195 = EDGE_CURVE ( 'NONE', #11174, #8071, #3958, .T. ) ;
#1196 = ADVANCED_FACE ( 'NONE', ( #9645 ), #5855, .T. ) ;
#1197 = CARTESIAN_POINT ( 'NONE',  ( 8.235329212248927888, -1.783486464602662691, 10.00000000000000000 ) ) ;
#1198 = CARTESIAN_POINT ( 'NONE',  ( -5.683926142426733108, 14.39978054689283660, 6.857782953271941950E-17 ) ) ;
#1199 = DIRECTION ( 'NONE',  ( -1.000000000000000000, -0.000000000000000000, 0.000000000000000000 ) ) ;
#1200 = CIRCLE ( 'NONE', #7650, 24.80000000000000071 ) ;
#1201 = CYLINDRICAL_SURFACE ( 'NONE', #7816, 9.599999999999997868 ) ;
#1202 = AXIS2_PLACEMENT_3D ( 'NONE', #1748, #5741, #6528 ) ;
#1203 = ORIENTED_EDGE ( 'NONE', *, *, #10173, .F. ) ;
#1204 = CIRCLE ( 'NONE', #2974, 24.80000000000000071 ) ;
#1205 = VECTOR ( 'NONE', #9593, 1000.000000000000000 ) ;
#1206 = ORIENTED_EDGE ( 'NONE', *, *, #5264, .F. ) ;
#1207 = EDGE_CURVE ( 'NONE', #1082, #8820, #9702, .T. ) ;
#1208 = DIRECTION ( 'NONE',  ( 0.000000000000000000, 0.000000000000000000, 1.000000000000000000 ) ) ;
#1209 = CARTESIAN_POINT ( 'NONE',  ( -10.00000000000000000, 0.000000000000000000, 0.000000000000000000 ) ) ;
#1210 = ADVANCED_FACE ( 'NONE', ( #10682 ), #1315, .T. ) ;
#1211 = PRESENTATION_LAYER_ASSIGNMENT (  '', '', ( #7661 ) ) ;
#1212 = CYLINDRICAL_SURFACE ( 'NONE', #2729, 24.80000000000000071 ) ;
#1213 = DIRECTION ( 'NONE',  ( -1.000000000000000000, -0.000000000000000000, 0.000000000000000000 ) ) ;
#1214 = CIRCLE ( 'NONE', #589, 24.80000000000000071 ) ;
#1215 = CARTESIAN_POINT ( 'NONE',  ( 10.39479819782869541, 2.258419626871296604, 3.747395293195558847E-16 ) ) ;
#1216 = AXIS2_PLACEMENT_3D ( 'NONE', #4607, #6379, #4547 ) ;
#1217 = CARTESIAN_POINT ( 'NONE',  ( 3.000000000000000888, -22.42251312757882786, 5.117118920208413968 ) ) ;
#1218 = ORIENTED_EDGE ( 'NONE', *, *, #1030, .F. ) ;
#1219 = ORIENTED_EDGE ( 'NONE', *, *, #8065, .T. ) ;
#1220 = DIRECTION ( 'NONE',  ( 0.000000000000000000, 1.000000000000000000, 0.000000000000000000 ) ) ;
#1221 = CARTESIAN_POINT ( 'NONE',  ( -15.85416723795449556, 2.087521067385502693, 10.00000000000000000 ) ) ;
#1222 = ORIENTED_EDGE ( 'NONE', *, *, #10564, .F. ) ;
#1223 = EDGE_CURVE ( 'NONE', #215, #12050, #9586, .T. ) ;
#1224 = DIRECTION ( 'NONE',  ( 0.000000000000000000, 0.000000000000000000, -1.000000000000000000 ) ) ;
#1225 = DIRECTION ( 'NONE',  ( 1.000000000000000000, 0.000000000000000000, -0.000000000000000000 ) ) ;
#1226 = DIRECTION ( 'NONE',  ( -1.000000000000000000, -0.000000000000000000, -0.000000000000000000 ) ) ;
#1227 = ORIENTED_EDGE ( 'NONE', *, *, #2172, .T. ) ;
#1228 = AXIS2_PLACEMENT_3D ( 'NONE', #11918, #11017, #4400 ) ;
#1229 = CARTESIAN_POINT ( 'NONE',  ( 0.000000000000000000, -22.54798042742717357, -0.4575788569254196636 ) ) ;
#1230 = DIRECTION ( 'NONE',  ( 0.000000000000000000, 0.000000000000000000, 1.000000000000000000 ) ) ;
#1231 = CARTESIAN_POINT ( 'NONE',  ( 10.35108484788238670, -9.702746953904560101, 6.857782953271941950E-17 ) ) ;
#1232 = VECTOR ( 'NONE', #6392, 1000.000000000000000 ) ;
#1233 = VERTEX_POINT ( 'NONE', #209 ) ;
#1234 = DIRECTION ( 'NONE',  ( 0.000000000000000000, 0.000000000000000000, 1.000000000000000000 ) ) ;
#1235 = ORIENTED_EDGE ( 'NONE', *, *, #11621, .T. ) ;
#1236 = LINE ( 'NONE', #5888, #9771 ) ;
#1237 = ORIENTED_EDGE ( 'NONE', *, *, #4685, .T. ) ;
#1238 = EDGE_CURVE ( 'NONE', #5236, #2346, #4017, .T. ) ;
#1239 = AXIS2_PLACEMENT_3D ( 'NONE', #2203, #10651, #7712 ) ;
#1240 = CARTESIAN_POINT ( 'NONE',  ( 10.50580257846854337, 1.391709641844861123, 10.00000000000000000 ) ) ;
#1241 = VECTOR ( 'NONE', #2002, 1000.000000000000000 ) ;
#1242 = AXIS2_PLACEMENT_3D ( 'NONE', #4961, #5070, #10585 ) ;
#1243 = FACE_OUTER_BOUND ( 'NONE', #10896, .T. ) ;
#1244 =( NAMED_UNIT ( * ) SI_UNIT ( $, .STERADIAN. ) SOLID_ANGLE_UNIT ( ) );
#1245 = VERTEX_POINT ( 'NONE', #6029 ) ;
#1246 = FACE_OUTER_BOUND ( 'NONE', #3018, .T. ) ;
#1247 = EDGE_CURVE ( 'NONE', #10823, #6189, #4140, .T. ) ;
#1248 = CARTESIAN_POINT ( 'NONE',  ( 3.000000000000000888, 22.54798042742718067, -0.4575788569252652871 ) ) ;
#1249 = CARTESIAN_POINT ( 'NONE',  ( 13.14573027368779456, 6.745762002080610387, 10.00000000000000000 ) ) ;
#1250 = CIRCLE ( 'NONE', #11408, 24.80000000000000071 ) ;
#1251 = DIRECTION ( 'NONE',  ( 0.000000000000000000, 0.000000000000000000, 1.000000000000000000 ) ) ;
#1252 = CARTESIAN_POINT ( 'NONE',  ( 2.839002905303027013, -15.63284973865750693, 3.747395293195558847E-16 ) ) ;
#1253 = DIRECTION ( 'NONE',  ( -1.000000000000000000, -0.000000000000000000, -0.000000000000000000 ) ) ;
#1254 = DIRECTION ( 'NONE',  ( 0.000000000000000000, 0.000000000000000000, 1.000000000000000000 ) ) ;
#1255 = ORIENTED_EDGE ( 'NONE', *, *, #3978, .F. ) ;
#1256 = VERTEX_POINT ( 'NONE', #1139 ) ;
#1257 = AXIS2_PLACEMENT_3D ( 'NONE', #9265, #10059, #1678 ) ;
#1258 = DIRECTION ( 'NONE',  ( -1.000000000000000000, -0.000000000000000000, -0.000000000000000000 ) ) ;
#1259 = CARTESIAN_POINT ( 'NONE',  ( 7.195390336726611658, 2.736402267197346028, 10.00000000000000000 ) ) ;
#1260 = CARTESIAN_POINT ( 'NONE',  ( 0.000000000000000000, -2.745295967526151237, 22.83456483164687967 ) ) ;
#1261 = CARTESIAN_POINT ( 'NONE',  ( -9.650762677556034674, -3.270672451565360461, 10.00000000000000000 ) ) ;
#1262 = CARTESIAN_POINT ( 'NONE',  ( 7.619603487155711008, -11.82824555707797387, 6.857782953271941950E-17 ) ) ;
#1263 = DIRECTION ( 'NONE',  ( -0.000000000000000000, -0.000000000000000000, -1.000000000000000000 ) ) ;
#1264 = CARTESIAN_POINT ( 'NONE',  ( 0.000000000000000000, 0.000000000000000000, 0.000000000000000000 ) ) ;
#1265 = ORIENTED_EDGE ( 'NONE', *, *, #1432, .F. ) ;
#1266 = ORIENTED_EDGE ( 'NONE', *, *, #3544, .F. ) ;
#1267 = DIRECTION ( 'NONE',  ( -1.000000000000000000, 0.000000000000000000, 0.000000000000000000 ) ) ;
#1268 = DIRECTION ( 'NONE',  ( 0.000000000000000000, 0.000000000000000000, -1.000000000000000000 ) ) ;
#1269 = LINE ( 'NONE', #4259, #1726 ) ;
#1270 = DIRECTION ( 'NONE',  ( -1.000000000000000000, -0.000000000000000000, -0.000000000000000000 ) ) ;
#1271 = CARTESIAN_POINT ( 'NONE',  ( -2.487495860704069361, -9.331140650584718088, 3.747395293195558847E-16 ) ) ;
#1272 = EDGE_CURVE ( 'NONE', #4610, #9844, #3527, .T. ) ;
#1273 = EDGE_CURVE ( 'NONE', #11632, #10794, #11562, .T. ) ;
#1274 = DIRECTION ( 'NONE',  ( -1.000000000000000000, 0.000000000000000000, 0.000000000000000000 ) ) ;
#1275 = ORIENTED_EDGE ( 'NONE', *, *, #5497, .T. ) ;
#1276 = ORIENTED_EDGE ( 'NONE', *, *, #2766, .T. ) ;
#1277 = ADVANCED_FACE ( 'NONE', ( #10558 ), #1201, .T. ) ;
#1278 = CARTESIAN_POINT ( 'NONE',  ( 0.000000000000000000, 23.00000000000000711, 0.000000000000000000 ) ) ;
#1279 = CARTESIAN_POINT ( 'NONE',  ( -14.76245309360257174, 5.834016798581408203, 10.00000000000000000 ) ) ;
#1280 = EDGE_LOOP ( 'NONE', ( #8265, #6299, #703, #8310 ) ) ;
#1281 = CYLINDRICAL_SURFACE ( 'NONE', #8779, 9.599999999999997868 ) ;
#1282 = CARTESIAN_POINT ( 'NONE',  ( 3.000000000000000888, 0.000000000000000000, 0.000000000000000000 ) ) ;
#1283 = DIRECTION ( 'NONE',  ( -1.000000000000000000, -0.000000000000000000, 0.000000000000000000 ) ) ;
#1284 = ORIENTED_EDGE ( 'NONE', *, *, #1273, .F. ) ;
#1285 = DIRECTION ( 'NONE',  ( 0.000000000000000000, 0.000000000000000000, 1.000000000000000000 ) ) ;
#1286 = CIRCLE ( 'NONE', #8126, 9.599999999999996092 ) ;
#1287 = DIRECTION ( 'NONE',  ( -1.000000000000000000, 0.000000000000000000, -0.000000000000000000 ) ) ;
#1288 = CARTESIAN_POINT ( 'NONE',  ( -12.80690425020131684, 9.177692349400029315, 6.857782953271941950E-17 ) ) ;
#1289 = ORIENTED_EDGE ( 'NONE', *, *, #6750, .F. ) ;
#1290 = DIRECTION ( 'NONE',  ( 0.000000000000000000, 0.000000000000000000, 1.000000000000000000 ) ) ;
#1291 = ORIENTED_EDGE ( 'NONE', *, *, #148, .F. ) ;
#1292 = LINE ( 'NONE', #11398, #10752 ) ;
#1293 = ORIENTED_EDGE ( 'NONE', *, *, #3442, .T. ) ;
#1294 = CIRCLE ( 'NONE', #7739, 19.99999999999999645 ) ;
#1295 = CARTESIAN_POINT ( 'NONE',  ( 0.6578947103914143391, -9.792230064638474119, 10.00000000000000000 ) ) ;
#1296 = ADVANCED_FACE ( 'NONE', ( #8612 ), #11359, .T. ) ;
#1297 = DIRECTION ( 'NONE',  ( 1.445602896647339163E-16, -1.000000000000000000, 0.000000000000000000 ) ) ;
#1298 = CYLINDRICAL_SURFACE ( 'NONE', #1709, 3.000000000000000000 ) ;
#1299 = CARTESIAN_POINT ( 'NONE',  ( 0.000000000000000000, 0.000000000000000000, 10.00000000000000000 ) ) ;
#1300 = CARTESIAN_POINT ( 'NONE',  ( 14.22875512193219372, -2.589574901423981501, 10.00000000000000000 ) ) ;
#1301 = EDGE_CURVE ( 'NONE', #3060, #5151, #1371, .T. ) ;
#1302 = AXIS2_PLACEMENT_3D ( 'NONE', #4835, #10338, #11387 ) ;
#1303 = LINE ( 'NONE', #2161, #52 ) ;
#1304 = CARTESIAN_POINT ( 'NONE',  ( 0.000000000000000000, -9.039786367038701087, -21.14796121233205284 ) ) ;
#1305 = DIRECTION ( 'NONE',  ( 1.000000000000000000, 0.000000000000000000, 0.000000000000000000 ) ) ;
#1306 = ORIENTED_EDGE ( 'NONE', *, *, #10319, .F. ) ;
#1307 = VERTEX_POINT ( 'NONE', #11838 ) ;
#1308 = ADVANCED_FACE ( 'NONE', ( #1500 ), #7924, .T. ) ;
#1309 = VERTEX_POINT ( 'NONE', #701 ) ;
#1310 = CARTESIAN_POINT ( 'NONE',  ( 3.000000000000000888, 5.135568396240030253, 21.96011696265493285 ) ) ;
#1311 = CARTESIAN_POINT ( 'NONE',  ( 3.000000000000000888, 21.58580335785676496, 6.532525787311040943 ) ) ;
#1312 = CARTESIAN_POINT ( 'NONE',  ( -9.352287007200070335, 3.176141031410558924, 10.00000000000000000 ) ) ;
#1313 = CARTESIAN_POINT ( 'NONE',  ( -8.739072045530900112, -14.04184524613900820, 6.857782953271941950E-17 ) ) ;
#1314 = DIRECTION ( 'NONE',  ( -1.000000000000000000, 0.000000000000000000, 0.000000000000000000 ) ) ;
#1315 = CYLINDRICAL_SURFACE ( 'NONE', #2574, 22.00000000000000000 ) ;
#1316 = ORIENTED_EDGE ( 'NONE', *, *, #32, .T. ) ;
#1317 = AXIS2_PLACEMENT_3D ( 'NONE', #9087, #7352, #7170 ) ;
#1318 = ORIENTED_EDGE ( 'NONE', *, *, #11892, .F. ) ;
#1319 = ORIENTED_EDGE ( 'NONE', *, *, #5767, .F. ) ;
#1320 = DIRECTION ( 'NONE',  ( 1.000000000000000000, -0.000000000000000000, -0.000000000000000000 ) ) ;
#1321 = CARTESIAN_POINT ( 'NONE',  ( 3.000000000000000888, -19.75591328264893676, 10.87771529938155268 ) ) ;
#1322 = CARTESIAN_POINT ( 'NONE',  ( 3.000000000000000888, 22.37663021667344054, 6.788022064062137595 ) ) ;
#1323 = CARTESIAN_POINT ( 'NONE',  ( 1.500000000000000444, 24.77821629063821973, 1.039229259764577140 ) ) ;
#1324 = AXIS2_PLACEMENT_3D ( 'NONE', #7096, #1479, #9126 ) ;
#1325 = CARTESIAN_POINT ( 'NONE',  ( 1.454091968623351327, 11.13059540125182423, 3.747395293195558847E-16 ) ) ;
#1326 = ADVANCED_BREP_SHAPE_REPRESENTATION ( '', ( #483, #8474 ), #1578 ) ;
#1327 = DIRECTION ( 'NONE',  ( 0.000000000000000000, 0.000000000000000000, 1.000000000000000000 ) ) ;
#1328 = ORIENTED_EDGE ( 'NONE', *, *, #3223, .T. ) ;
#1329 = VERTEX_POINT ( 'NONE', #6994 ) ;
#1330 =( LENGTH_UNIT ( ) NAMED_UNIT ( * ) SI_UNIT ( .MILLI., .METRE. ) );
#1331 = CARTESIAN_POINT ( 'NONE',  ( -12.98359546555290045, 0.8565524458112724338, 10.00000000000000000 ) ) ;
#1332 = ORIENTED_EDGE ( 'NONE', *, *, #11096, .T. ) ;
#1333 = AXIS2_PLACEMENT_3D ( 'NONE', #4205, #465, #10569 ) ;
#1334 = CARTESIAN_POINT ( 'NONE',  ( 3.000000000000000888, 21.97702544527757951, 6.779701584702809924 ) ) ;
#1335 = DIRECTION ( 'NONE',  ( -1.000000000000000000, -0.000000000000000000, -0.000000000000000000 ) ) ;
#1336 = UNCERTAINTY_MEASURE_WITH_UNIT (LENGTH_MEASURE( 1.000000000000000082E-05 ), #7812, 'distance_accuracy_value', 'NONE');
#1337 = DIRECTION ( 'NONE',  ( -1.000000000000000000, 0.000000000000000000, 0.000000000000000000 ) ) ;
#1338 = ORIENTED_EDGE ( 'NONE', *, *, #11596, .F. ) ;
#1339 = ADVANCED_FACE ( 'NONE', ( #3337 ), #9092, .T. ) ;
#1340 = CARTESIAN_POINT ( 'NONE',  ( 0.000000000000000000, -17.71842311621541555, 17.35216073792434699 ) ) ;
#1341 = EDGE_CURVE ( 'NONE', #10120, #5082, #7246, .T. ) ;
#1342 = EDGE_CURVE ( 'NONE', #11577, #1307, #3132, .T. ) ;
#1343 = FACE_OUTER_BOUND ( 'NONE', #7607, .T. ) ;
#1344 = CARTESIAN_POINT ( 'NONE',  ( -1.916691774771271284, -10.52688368019216014, 6.857782953271941950E-17 ) ) ;
#1345 = AXIS2_PLACEMENT_3D ( 'NONE', #8106, #6337, #1553 ) ;
#1346 = EDGE_LOOP ( 'NONE', ( #829, #800, #7562, #3730 ) ) ;
#1347 = CARTESIAN_POINT ( 'NONE',  ( 3.000000000000000888, 19.29833442572359559, 11.67026512804553562 ) ) ;
#1348 = ORIENTED_EDGE ( 'NONE', *, *, #833, .F. ) ;
#1349 = LINE ( 'NONE', #11686, #10573 ) ;
#1350 = EDGE_LOOP ( 'NONE', ( #7731, #8140, #8311, #7645 ) ) ;
#1351 = CARTESIAN_POINT ( 'NONE',  ( -7.812220363924760491, -5.053636123081433951, 10.00000000000000000 ) ) ;
#1352 = EDGE_CURVE ( 'NONE', #9137, #10458, #1628, .T. ) ;
#1353 = VECTOR ( 'NONE', #9531, 1000.000000000000000 ) ;
#1354 = LINE ( 'NONE', #10716, #5395 ) ;
#1355 = SURFACE_SIDE_STYLE ('',( #9737 ) ) ;
#1356 = AXIS2_PLACEMENT_3D ( 'NONE', #6773, #4026, #228 ) ;
#1357 = DIRECTION ( 'NONE',  ( 0.000000000000000000, 0.000000000000000000, 1.000000000000000000 ) ) ;
#1358 = CARTESIAN_POINT ( 'NONE',  ( 3.000000000000000888, 8.645255683529006419, 23.24434456306327590 ) ) ;
#1359 = CARTESIAN_POINT ( 'NONE',  ( 7.334967666341840165, -8.371827447635059372, 10.00000000000000000 ) ) ;
#1360 = LINE ( 'NONE', #6075, #11377 ) ;
#1361 = CARTESIAN_POINT ( 'NONE',  ( 11.04976219204102783, -11.79656285006036676, 3.747395293195558847E-16 ) ) ;
#1362 = CARTESIAN_POINT ( 'NONE',  ( 0.000000000000000000, 15.80756504416690866, 19.10918332567963773 ) ) ;
#1363 = ADVANCED_FACE ( 'NONE', ( #5296 ), #578, .T. ) ;
#1364 = VERTEX_POINT ( 'NONE', #3408 ) ;
#1365 = CYLINDRICAL_SURFACE ( 'NONE', #10553, 9.599999999999997868 ) ;
#1366 = AXIS2_PLACEMENT_3D ( 'NONE', #6949, #2370, #8744 ) ;
#1367 = VERTEX_POINT ( 'NONE', #2539 ) ;
#1368 = ORIENTED_EDGE ( 'NONE', *, *, #9518, .F. ) ;
#1369 = EDGE_CURVE ( 'NONE', #8857, #9360, #4251, .T. ) ;
#1370 = FACE_OUTER_BOUND ( 'NONE', #11080, .T. ) ;
#1371 = CIRCLE ( 'NONE', #6829, 5.000000000000000000 ) ;
#1372 = DIRECTION ( 'NONE',  ( 0.000000000000000000, 0.4067366430757948792, 0.9135454576426033091 ) ) ;
#1373 = CIRCLE ( 'NONE', #583, 24.80000000000000071 ) ;
#1374 = DIRECTION ( 'NONE',  ( 1.000000000000000000, 0.000000000000000000, 0.000000000000000000 ) ) ;
#1375 = CARTESIAN_POINT ( 'NONE',  ( 2.084091085258986897, 8.931495281877387171, 10.00000000000000000 ) ) ;
#1376 = CARTESIAN_POINT ( 'NONE',  ( 2.469054641153893837, -10.61194774715159284, 6.857782953271941950E-17 ) ) ;
#1377 = CARTESIAN_POINT ( 'NONE',  ( 3.000000000000000888, 0.000000000000000000, 0.000000000000000000 ) ) ;
#1378 = CARTESIAN_POINT ( 'NONE',  ( 0.000000000000000000, 16.45023496161665122, 15.42759117534391322 ) ) ;
#1379 = ORIENTED_EDGE ( 'NONE', *, *, #9289, .F. ) ;
#1380 = ORIENTED_EDGE ( 'NONE', *, *, #4966, .T. ) ;
#1381 = AXIS2_PLACEMENT_3D ( 'NONE', #9537, #976, #10331 ) ;
#1382 = AXIS2_PLACEMENT_3D ( 'NONE', #12007, #934, #3687 ) ;
#1383 = VERTEX_POINT ( 'NONE', #7979 ) ;
#1384 = ADVANCED_FACE ( 'NONE', ( #10869 ), #10064, .T. ) ;
#1385 = LINE ( 'NONE', #11548, #1205 ) ;
#1386 = DIRECTION ( 'NONE',  ( -1.000000000000000000, -0.000000000000000000, -0.000000000000000000 ) ) ;
#1387 = LINE ( 'NONE', #1323, #3883 ) ;
#1388 = AXIS2_PLACEMENT_3D ( 'NONE', #8280, #12005, #8523 ) ;
#1389 = EDGE_CURVE ( 'NONE', #843, #3060, #7055, .T. ) ;
#1390 = CIRCLE ( 'NONE', #3157, 9.599999999999996092 ) ;
#1391 = CARTESIAN_POINT ( 'NONE',  ( -0.3758430365714711674, 11.29677535215814110, 3.747395293195558847E-16 ) ) ;
#1392 = VECTOR ( 'NONE', #9347, 1000.000000000000000 ) ;
#1393 = DIRECTION ( 'NONE',  ( -0.000000000000000000, 0.000000000000000000, 1.000000000000000000 ) ) ;
#1394 = DIRECTION ( 'NONE',  ( -1.000000000000000000, 0.000000000000000000, 0.000000000000000000 ) ) ;
#1395 = ORIENTED_EDGE ( 'NONE', *, *, #8378, .F. ) ;
#1396 = ORIENTED_EDGE ( 'NONE', *, *, #5019, .F. ) ;
#1397 = ITEM_DEFINED_TRANSFORMATION ( 'NONE', 'NONE', #5688,  #8474 ) ;
#1398 = CARTESIAN_POINT ( 'NONE',  ( 11.20109743375192224, 9.815261043520028039, 10.00000000000000000 ) ) ;
#1399 = AXIS2_PLACEMENT_3D ( 'NONE', #4070, #511, #7050 ) ;
#1400 = ORIENTED_EDGE ( 'NONE', *, *, #10170, .F. ) ;
#1401 = FACE_OUTER_BOUND ( 'NONE', #3208, .T. ) ;
#1402 = FACE_OUTER_BOUND ( 'NONE', #11929, .T. ) ;
#1403 = AXIS2_PLACEMENT_3D ( 'NONE', #8748, #10457, #11318 ) ;
#1404 = DIRECTION ( 'NONE',  ( -0.000000000000000000, -0.000000000000000000, 1.000000000000000000 ) ) ;
#1405 = ORIENTED_EDGE ( 'NONE', *, *, #370, .F. ) ;
#1406 = CARTESIAN_POINT ( 'NONE',  ( 0.000000000000000000, 1.039229259764488544, 24.77821629063822328 ) ) ;
#1407 = DIRECTION ( 'NONE',  ( -1.000000000000000000, 0.000000000000000000, 0.000000000000000000 ) ) ;
#1408 = CARTESIAN_POINT ( 'NONE',  ( 7.605204090343169909, 4.385345779697310320, 6.857782953271941950E-17 ) ) ;
#1409 = VECTOR ( 'NONE', #10085, 1000.000000000000000 ) ;
#1410 = ORIENTED_EDGE ( 'NONE', *, *, #4874, .T. ) ;
#1411 = CARTESIAN_POINT ( 'NONE',  ( 0.000000000000000000, 13.79477846460820700, -18.40266524480574972 ) ) ;
#1412 = DIRECTION ( 'NONE',  ( 0.000000000000000000, 0.000000000000000000, 1.000000000000000000 ) ) ;
#1413 = ORIENTED_EDGE ( 'NONE', *, *, #3339, .T. ) ;
#1414 = EDGE_CURVE ( 'NONE', #2229, #1487, #2418, .T. ) ;
#1415 = CARTESIAN_POINT ( 'NONE',  ( -11.32214898804313208, 3.633524203737720448, 10.00000000000000000 ) ) ;
#1416 = AXIS2_PLACEMENT_3D ( 'NONE', #10027, #9910, #1524 ) ;
#1417 = ORIENTED_EDGE ( 'NONE', *, *, #748, .F. ) ;
#1418 = DIRECTION ( 'NONE',  ( -1.000000000000000000, 0.000000000000000000, 0.000000000000000000 ) ) ;
#1419 = VERTEX_POINT ( 'NONE', #11897 ) ;
#1420 = CARTESIAN_POINT ( 'NONE',  ( 3.000000000000000888, 0.000000000000000000, 0.000000000000000000 ) ) ;
#1421 = CARTESIAN_POINT ( 'NONE',  ( 0.000000000000000000, -9.589108953447752270, -20.41249101028221702 ) ) ;
#1422 = CARTESIAN_POINT ( 'NONE',  ( 4.764169229607557732, 7.652272242165495619, 10.00000000000000000 ) ) ;
#1423 = CARTESIAN_POINT ( 'NONE',  ( 0.000000000000000000, 18.40266524480607657, -13.79477846460777357 ) ) ;
#1424 = CARTESIAN_POINT ( 'NONE',  ( 5.172292865810426576, -11.91455349003027564, 3.747395293195558847E-16 ) ) ;
#1425 = EDGE_CURVE ( 'NONE', #3560, #7905, #5417, .T. ) ;
#1426 = DIRECTION ( 'NONE',  ( 0.000000000000000000, 0.5000000000000011102, -0.8660254037844381525 ) ) ;
#1427 = AXIS2_PLACEMENT_3D ( 'NONE', #6376, #4415, #8147 ) ;
#1428 = DIRECTION ( 'NONE',  ( 0.000000000000000000, 0.1045284632676469622, 0.9945218953682738450 ) ) ;
#1429 = EDGE_CURVE ( 'NONE', #8745, #5789, #4378, .T. ) ;
#1430 = VERTEX_POINT ( 'NONE', #7117 ) ;
#1431 = CIRCLE ( 'NONE', #9634, 9.599999999999997868 ) ;
#1432 = EDGE_CURVE ( 'NONE', #10038, #401, #4311, .T. ) ;
#1433 = DIRECTION ( 'NONE',  ( 1.000000000000000000, 0.000000000000000000, 0.000000000000000000 ) ) ;
#1434 = ORIENTED_EDGE ( 'NONE', *, *, #9981, .T. ) ;
#1435 = CIRCLE ( 'NONE', #9067, 24.80000000000000071 ) ;
#1436 = CARTESIAN_POINT ( 'NONE',  ( 0.000000000000000000, 0.000000000000000000, 0.000000000000000000 ) ) ;
#1437 = DIRECTION ( 'NONE',  ( 0.000000000000000000, -0.8660254037844328234, -0.5000000000000099920 ) ) ;
#1438 = CARTESIAN_POINT ( 'NONE',  ( 5.508953106497951779, 1.454581011951755043, 10.00000000000000000 ) ) ;
#1439 = CARTESIAN_POINT ( 'NONE',  ( 7.334967666341834835, -8.371827447635054043, 6.857782953271941950E-17 ) ) ;
#1440 = CARTESIAN_POINT ( 'NONE',  ( 3.000000000000000888, 4.135161237383582211, 24.45282072769602166 ) ) ;
#1441 = CARTESIAN_POINT ( 'NONE',  ( 1.500000000000000444, 19.10918332567978695, -15.80756504416671859 ) ) ;
#1442 = ORIENTED_EDGE ( 'NONE', *, *, #10393, .T. ) ;
#1443 = ORIENTED_EDGE ( 'NONE', *, *, #10130, .F. ) ;
#1444 = VECTOR ( 'NONE', #11775, 1000.000000000000000 ) ;
#1445 = VERTEX_POINT ( 'NONE', #9939 ) ;
#1446 = CARTESIAN_POINT ( 'NONE',  ( -1.872083171988683015, 14.23747171912756393, 10.00000000000000000 ) ) ;
#1447 = FILL_AREA_STYLE ('',( #1505 ) ) ;
#1448 = CARTESIAN_POINT ( 'NONE',  ( 3.000000000000000888, 6.532525787311267429, -21.58580335785669746 ) ) ;
#1449 = AXIS2_PLACEMENT_3D ( 'NONE', #10163, #9073, #4355 ) ;
#1450 = CARTESIAN_POINT ( 'NONE',  ( 6.723006375386860967, 3.907299473125124489, 3.747395293195558847E-16 ) ) ;
#1451 = EDGE_CURVE ( 'NONE', #2557, #11577, #3745, .T. ) ;
#1452 = DIRECTION ( 'NONE',  ( -1.000000000000000000, 0.000000000000000000, 0.000000000000000000 ) ) ;
#1453 = DIRECTION ( 'NONE',  ( 1.000000000000000000, 0.000000000000000000, 0.000000000000000000 ) ) ;
#1454 = VERTEX_POINT ( 'NONE', #10988 ) ;
#1455 = ORIENTED_EDGE ( 'NONE', *, *, #8279, .F. ) ;
#1456 = CARTESIAN_POINT ( 'NONE',  ( -12.72059027619867955, -3.407653011836159873, 10.00000000000000000 ) ) ;
#1457 = ORIENTED_EDGE ( 'NONE', *, *, #6577, .T. ) ;
#1458 = CARTESIAN_POINT ( 'NONE',  ( 1.499999999999999556, 6.168200451485757796, 24.02068490260614908 ) ) ;
#1459 = DIRECTION ( 'NONE',  ( 0.000000000000000000, 0.000000000000000000, 1.000000000000000000 ) ) ;
#1460 = CARTESIAN_POINT ( 'NONE',  ( 3.000000000000000888, 9.128825345753028842, 23.05871956130125255 ) ) ;
#1461 = ADVANCED_FACE ( 'NONE', ( #6342 ), #1683, .T. ) ;
#1462 = UNCERTAINTY_MEASURE_WITH_UNIT (LENGTH_MEASURE( 1.000000000000000082E-05 ), #12067, 'distance_accuracy_value', 'NONE');
#1463 = DIRECTION ( 'NONE',  ( 0.000000000000000000, 0.5877852522924742473, -0.8090169943749466741 ) ) ;
#1464 = ORIENTED_EDGE ( 'NONE', *, *, #7745, .T. ) ;
#1465 = CARTESIAN_POINT ( 'NONE',  ( 0.000000000000000000, 0.000000000000000000, 0.000000000000000000 ) ) ;
#1466 = LINE ( 'NONE', #6847, #4148 ) ;
#1467 = CARTESIAN_POINT ( 'NONE',  ( -8.209791827104812256, -6.297951179201748850, 6.857782953271941950E-17 ) ) ;
#1468 = VERTEX_POINT ( 'NONE', #14 ) ;
#1469 = CARTESIAN_POINT ( 'NONE',  ( 0.000000000000000000, 0.000000000000000000, 0.000000000000000000 ) ) ;
#1470 = ORIENTED_EDGE ( 'NONE', *, *, #3009, .F. ) ;
#1471 = DIRECTION ( 'NONE',  ( -1.000000000000000000, 0.000000000000000000, -0.000000000000000000 ) ) ;
#1472 = ORIENTED_EDGE ( 'NONE', *, *, #2415, .T. ) ;
#1473 = CARTESIAN_POINT ( 'NONE',  ( -3.141381368647836236, 10.98006565327106543, 10.00000000000000000 ) ) ;
#1474 = VERTEX_POINT ( 'NONE', #5660 ) ;
#1475 = DIRECTION ( 'NONE',  ( 0.000000000000000000, 0.000000000000000000, 1.000000000000000000 ) ) ;
#1476 = CIRCLE ( 'NONE', #5971, 3.500000000000000000 ) ;
#1477 = PRESENTATION_STYLE_ASSIGNMENT (( #10268 ) ) ;
#1478 = EDGE_LOOP ( 'NONE', ( #12078, #1615, #9783, #231 ) ) ;
#1479 = DIRECTION ( 'NONE',  ( -1.000000000000000000, 0.000000000000000000, 0.000000000000000000 ) ) ;
#1480 = CARTESIAN_POINT ( 'NONE',  ( 3.000000000000000888, 22.54798042742717712, 0.4575788569255671012 ) ) ;
#1481 = CARTESIAN_POINT ( 'NONE',  ( 6.242895496889244278, -5.302832405932367266, 10.00000000000000000 ) ) ;
#1482 = CYLINDRICAL_SURFACE ( 'NONE', #10001, 4.000000000000000000 ) ;
#1483 = CARTESIAN_POINT ( 'NONE',  ( 13.29800827116429573, 3.099979537169514909, 3.747395293195558847E-16 ) ) ;
#1484 = CARTESIAN_POINT ( 'NONE',  ( 0.000000000000000000, 5.135568396240338451, -21.96011696265485824 ) ) ;
#1485 = AXIS2_PLACEMENT_3D ( 'NONE', #6008, #9736, #5088 ) ;
#1486 = DIRECTION ( 'NONE',  ( 0.000000000000000000, 0.000000000000000000, 1.000000000000000000 ) ) ;
#1487 = VERTEX_POINT ( 'NONE', #8231 ) ;
#1488 = EDGE_CURVE ( 'NONE', #5509, #8343, #9992, .T. ) ;
#1489 = CARTESIAN_POINT ( 'NONE',  ( 3.000000000000000888, -16.45023496161654819, -15.42759117534402513 ) ) ;
#1490 =( NAMED_UNIT ( * ) SI_UNIT ( $, .STERADIAN. ) SOLID_ANGLE_UNIT ( ) );
#1491 = VERTEX_POINT ( 'NONE', #82 ) ;
#1492 = EDGE_CURVE ( 'NONE', #10594, #10386, #9022, .T. ) ;
#1493 = DIRECTION ( 'NONE',  ( 1.000000000000000000, 0.000000000000000000, -0.000000000000000000 ) ) ;
#1494 = EDGE_CURVE ( 'NONE', #10107, #3562, #11343, .T. ) ;
#1495 = DIRECTION ( 'NONE',  ( -1.000000000000000000, -0.000000000000000000, 0.000000000000000000 ) ) ;
#1496 = DIRECTION ( 'NONE',  ( 1.000000000000000000, 0.000000000000000000, -0.000000000000000000 ) ) ;
#1497 = CARTESIAN_POINT ( 'NONE',  ( -9.977213461302312680, -1.645879626164740817, 6.857782953271941950E-17 ) ) ;
#1498 = CARTESIAN_POINT ( 'NONE',  ( 17.49999999999999645, 0.000000000000000000, 6.857782953271941950E-17 ) ) ;
#1499 = EDGE_CURVE ( 'NONE', #8706, #9548, #782, .T. ) ;
#1500 = FACE_OUTER_BOUND ( 'NONE', #5662, .T. ) ;
#1501 = ORIENTED_EDGE ( 'NONE', *, *, #218, .F. ) ;
#1502 = ORIENTED_EDGE ( 'NONE', *, *, #4060, .T. ) ;
#1503 = CARTESIAN_POINT ( 'NONE',  ( 1.050035089571674352, -12.78847817906846451, 10.00000000000000000 ) ) ;
#1504 = ADVANCED_FACE ( 'NONE', ( #2721 ), #3827, .T. ) ;
#1505 = FILL_AREA_STYLE_COLOUR ( '', #10720 ) ;
#1506 = CARTESIAN_POINT ( 'NONE',  ( 0.000000000000000000, 0.000000000000000000, 0.000000000000000000 ) ) ;
#1507 = B_SPLINE_CURVE_WITH_KNOTS ( 'NONE', 3,
 ( #9651, #11485, #8796, #2183, #3107, #6769, #6824, #10566, #3170, #342, #6942, #10633, #9834, #11660, #3277, #4881, #8916, #1632, #5421, #4503, #6283, #3590, #8116, #582, #1689, #522, #8052, #6347, #10814, #4257, #3415, #10927, #2424, #4440, #763, #7300, #706, #10995, #1446, #6164, #2612, #8172, #4319, #11901, #9149, #4384, #11962, #2667, #7983, #10006, #5370, #3528, #10069, #11052, #8238, #5181, #6398, #2545, #8971, #9892, #9096, #10874, #11787, #11720, #1503, #7123, #650, #1564, #7242, #5238, #3344, #7061, #2485, #6219, #9946, #5303, #9037, #11843, #3472, #7181, #1742, #1021, #832, #10192, #7496, #9215, #7554, #4629, #5733, #10371, #1993, #8360, #2853, #892, #1928, #9460, #9335, #5664, #12082, #1809, #10255, #951, #26, #11241, #1077, #6522, #4569, #4808, #3648, #11109, #3887, #11179, #8491, #6634, #8299, #5548, #4688, #2912, #9395, #1867, #12023, #11295, #5478, #5604, #8547, #4753, #88, #3706, #3834, #142, #7429, #8426, #2792, #2727, #6576, #7609, #11353, #2977, #10124, #7365, #6458, #10309, #9277, #3774, #6874, #5908, #10551, #9638, #10435, #3094, #6697, #1259, #11419, #6813, #5791, #1133, #10616, #4867, #2054, #7736, #4990, #5850, #9516, #8605, #202, #270, #8727, #8669, #329, #3953, #2168, #4068, #4012, #1191, #7798, #2110, #7679, #3039, #6757, #4931, #11533, #10494, #11474, #3156, #9578, #7134, #4453, #2624, #4271, #6176, #663, #11010, #10019, #6232, #5193, #10079, #5319, #10885, #3485, #9903, #3604, #4331, #9108, #6356, #8986, #9960, #3427, #10827 ),
 .UNSPECIFIED., .F., .F.,
 ( 4, 2, 2, 2, 2, 2, 2, 2, 2, 2, 2, 2, 2, 2, 2, 2, 2, 2, 2, 2, 2, 2, 2, 2, 2, 2, 2, 2, 2, 2, 2, 2, 2, 2, 2, 2, 2, 2, 2, 2, 2, 2, 2, 2, 2, 2, 2, 2, 2, 2, 2, 2, 2, 2, 2, 2, 2, 2, 2, 2, 2, 2, 2, 2, 2, 2, 2, 2, 2, 2, 2, 2, 2, 2, 2, 2, 2, 2, 2, 2, 2, 2, 2, 2, 2, 2, 2, 2, 2, 2, 2, 2, 2, 2, 2, 2, 2, 2, 2, 2, 2, 2, 2, 4 ),
 ( 0.000000000000000000, 0.007812500000000000000, 0.01562500000000000000, 0.02343750000000000000, 0.03125000000000000000, 0.03906250000000000000, 0.04687500000000000000, 0.05468750000000000000, 0.06250000000000000000, 0.07031250000000000000, 0.07812500000000000000, 0.08593750000000000000, 0.09375000000000000000, 0.1015624999999999861, 0.1093750000000000000, 0.1171875000000000000, 0.1250000000000000000, 0.1328125000000000000, 0.1406250000000000000, 0.1484375000000000000, 0.1562500000000000000, 0.1640624999999999722, 0.1718750000000000000, 0.1796875000000000000, 0.1875000000000000000, 0.1953125000000000000, 0.2031249999999999722, 0.2109375000000000000, 0.2187500000000000000, 0.2265625000000000000, 0.2343750000000000000, 0.2421875000000000000, 0.2500000000000000000, 0.2578125000000000000, 0.2656250000000000000, 0.2734375000000000000, 0.2812500000000000000, 0.2890625000000000000, 0.2968750000000000000, 0.3046875000000000000, 0.3125000000000000000, 0.3203125000000000000, 0.3281249999999999445, 0.3359375000000000000, 0.3437500000000000000, 0.3515625000000000000, 0.3593750000000000000, 0.3671874999999999445, 0.3750000000000000000, 0.3828125000000000000, 0.3906250000000000000, 0.3984375000000000000, 0.4062499999999999445, 0.4140625000000000000, 0.4218750000000000000, 0.4296875000000000000, 0.4375000000000000000, 0.4453125000000000000, 0.4531250000000000000, 0.4609375000000000000, 0.4687500000000000000, 0.4765625000000000000, 0.4843750000000000000, 0.4921875000000000000, 0.5000000000000000000, 0.5078125000000000000, 0.5156250000000000000, 0.5234375000000000000, 0.5312500000000000000, 0.5390625000000000000, 0.5468750000000000000, 0.5546875000000000000, 0.5625000000000000000, 0.5703125000000000000, 0.5781250000000000000, 0.5859375000000000000, 0.5937500000000000000, 0.6015625000000000000, 0.6093750000000000000, 0.6171874999999998890, 0.6250000000000000000, 0.6328125000000000000, 0.6406250000000000000, 0.6484375000000000000, 0.6562499999999998890, 0.6640625000000000000, 0.6718750000000000000, 0.6796875000000000000, 0.6875000000000000000, 0.6953124999999998890, 0.7031250000000000000, 0.7109375000000000000, 0.7187500000000000000, 0.7265625000000000000, 0.7343749999999998890, 0.7421875000000000000, 0.7500000000000000000, 0.7656250000000000000, 0.7812500000000000000, 0.7968750000000000000, 0.8124999999999998890, 0.8281250000000000000, 0.8437500000000000000, 0.8499999999999999778 ),
 .UNSPECIFIED. ) ;
#1508 = CARTESIAN_POINT ( 'NONE',  ( -5.862605222286285667, -1.923479314576677535, 3.747395293195558847E-16 ) ) ;
#1509 = CARTESIAN_POINT ( 'NONE',  ( 3.000000000000000888, 17.06259499759944021, 14.74749645580017088 ) ) ;
#1510 = DIRECTION ( 'NONE',  ( -1.000000000000000000, -0.000000000000000000, -0.000000000000000000 ) ) ;
#1511 = ORIENTED_EDGE ( 'NONE', *, *, #6007, .T. ) ;
#1512 = ORIENTED_EDGE ( 'NONE', *, *, #6587, .T. ) ;
#1513 = ADVANCED_FACE ( 'NONE', ( #10185 ), #8484, .T. ) ;
#1514 = PRODUCT_CONTEXT ( 'NONE', #2788, 'mechanical' ) ;
#1515 = CARTESIAN_POINT ( 'NONE',  ( 5.343773788080183884, 10.82393792025544421, 10.00000000000000000 ) ) ;
#1516 = ORIENTED_EDGE ( 'NONE', *, *, #1352, .F. ) ;
#1517 = DIRECTION ( 'NONE',  ( -1.000000000000000000, -0.000000000000000000, 0.000000000000000000 ) ) ;
#1518 = DIRECTION ( 'NONE',  ( -1.000000000000000000, 0.000000000000000000, -0.000000000000000000 ) ) ;
#1519 = DIRECTION ( 'NONE',  ( -1.000000000000000000, -0.000000000000000000, -0.000000000000000000 ) ) ;
#1520 = EDGE_CURVE ( 'NONE', #7759, #7087, #4731, .T. ) ;
#1521 = CARTESIAN_POINT ( 'NONE',  ( 3.000000000000000888, 0.000000000000000000, 0.000000000000000000 ) ) ;
#1522 = ORIENTED_EDGE ( 'NONE', *, *, #6465, .T. ) ;
#1523 = CYLINDRICAL_SURFACE ( 'NONE', #7282, 9.599999999999997868 ) ;
#1524 = DIRECTION ( 'NONE',  ( 0.000000000000000000, -0.5877852522924799095, 0.8090169943749425663 ) ) ;
#1525 = CARTESIAN_POINT ( 'NONE',  ( 2.578468386369129117, 11.91291369680096857, 6.857782953271941950E-17 ) ) ;
#1526 = EDGE_CURVE ( 'NONE', #10640, #4392, #2950, .T. ) ;
#1527 = DIRECTION ( 'NONE',  ( 0.000000000000000000, 0.000000000000000000, -1.000000000000000000 ) ) ;
#1528 = AXIS2_PLACEMENT_3D ( 'NONE', #2441, #8255, #6180 ) ;
#1529 = CARTESIAN_POINT ( 'NONE',  ( 3.000000000000000888, 14.74749645580011226, 17.06259499759949705 ) ) ;
#1530 = ORIENTED_EDGE ( 'NONE', *, *, #2012, .T. ) ;
#1531 = CARTESIAN_POINT ( 'NONE',  ( 3.656769781543558917, 7.172433557890307121, 10.00000000000000000 ) ) ;
#1532 = ORIENTED_EDGE ( 'NONE', *, *, #10939, .T. ) ;
#1533 = CARTESIAN_POINT ( 'NONE',  ( 0.000000000000000000, 0.000000000000000000, 0.000000000000000000 ) ) ;
#1534 = LINE ( 'NONE', #5619, #5659 ) ;
#1535 = ORIENTED_EDGE ( 'NONE', *, *, #10921, .F. ) ;
#1536 = LINE ( 'NONE', #3443, #939 ) ;
#1537 = AXIS2_PLACEMENT_3D ( 'NONE', #9337, #28, #7497 ) ;
#1538 = CARTESIAN_POINT ( 'NONE',  ( 0.000000000000000000, -7.402892494506152943, -21.30300407174369681 ) ) ;
#1539 = CARTESIAN_POINT ( 'NONE',  ( -5.125696908148163367, -9.212757455310160992, 10.00000000000000000 ) ) ;
#1540 = ADVANCED_FACE ( 'NONE', ( #1802 ), #888, .T. ) ;
#1541 = CARTESIAN_POINT ( 'NONE',  ( 3.000000000000000888, 0.000000000000000000, 0.000000000000000000 ) ) ;
#1542 = CARTESIAN_POINT ( 'NONE',  ( 3.885483365683944257, 13.62125166200964976, 3.747395293195558847E-16 ) ) ;
#1543 = CYLINDRICAL_SURFACE ( 'NONE', #10955, 9.599999999999997868 ) ;
#1544 = ORIENTED_EDGE ( 'NONE', *, *, #10259, .F. ) ;
#1545 = ORIENTED_EDGE ( 'NONE', *, *, #1526, .F. ) ;
#1546 = DIRECTION ( 'NONE',  ( 0.000000000000000000, 0.000000000000000000, 1.000000000000000000 ) ) ;
#1547 = ORIENTED_EDGE ( 'NONE', *, *, #5991, .F. ) ;
#1548 = MECHANICAL_DESIGN_GEOMETRIC_PRESENTATION_REPRESENTATION (  '', ( #9368 ), #5064 ) ;
#1549 = DIRECTION ( 'NONE',  ( -1.000000000000000000, -0.000000000000000000, -0.000000000000000000 ) ) ;
#1550 = CARTESIAN_POINT ( 'NONE',  ( 0.000000000000000000, 0.000000000000000000, 0.000000000000000000 ) ) ;
#1551 = DIRECTION ( 'NONE',  ( 0.000000000000000000, 0.000000000000000000, 1.000000000000000000 ) ) ;
#1552 = EDGE_LOOP ( 'NONE', ( #6559, #8552, #1255, #3557 ) ) ;
#1553 = DIRECTION ( 'NONE',  ( 0.000000000000000000, 0.5877852522924742473, -0.8090169943749467851 ) ) ;
#1554 = CARTESIAN_POINT ( 'NONE',  ( 0.000000000000000000, 0.000000000000000000, -5.000000000000000000 ) ) ;
#1555 = CARTESIAN_POINT ( 'NONE',  ( -6.829322889802586616, -2.192323464439263514, 10.00000000000000000 ) ) ;
#1556 = CIRCLE ( 'NONE', #9955, 24.80000000000000071 ) ;
#1557 = CARTESIAN_POINT ( 'NONE',  ( -8.209791827104812256, -6.297951179201748850, 6.857782953271941950E-17 ) ) ;
#1558 = CARTESIAN_POINT ( 'NONE',  ( 3.000000000000000888, 0.000000000000000000, 0.000000000000000000 ) ) ;
#1559 = DIRECTION ( 'NONE',  ( 0.000000000000000000, 0.8090169943749485615, -0.5877852522924714718 ) ) ;
#1560 = ORIENTED_EDGE ( 'NONE', *, *, #7387, .F. ) ;
#1561 = ORIENTED_EDGE ( 'NONE', *, *, #1499, .T. ) ;
#1562 = VERTEX_POINT ( 'NONE', #4497 ) ;
#1563 = AXIS2_PLACEMENT_3D ( 'NONE', #516, #2481, #6095 ) ;
#1564 = CARTESIAN_POINT ( 'NONE',  ( -4.054747718262374789, -11.96785467447666029, 10.00000000000000000 ) ) ;
#1565 = ADVANCED_FACE ( 'NONE', ( #7489 ), #10304, .F. ) ;
#1566 = AXIS2_PLACEMENT_3D ( 'NONE', #9954, #714, #6293 ) ;
#1567 = CARTESIAN_POINT ( 'NONE',  ( 0.000000000000000000, -9.667200211209685534, -20.86861857134744014 ) ) ;
#1568 = FACE_OUTER_BOUND ( 'NONE', #1601, .T. ) ;
#1569 = CARTESIAN_POINT ( 'NONE',  ( -5.704017324792769905, 1.489539271746818772, 3.747395293195558847E-16 ) ) ;
#1570 = AXIS2_PLACEMENT_3D ( 'NONE', #8663, #2226, #11525 ) ;
#1571 = LINE ( 'NONE', #3421, #10572 ) ;
#1572 = CIRCLE ( 'NONE', #10991, 22.99899999999999523 ) ;
#1573 = AXIS2_PLACEMENT_3D ( 'NONE', #10974, #2594, #6329 ) ;
#1574 = EDGE_CURVE ( 'NONE', #8389, #10578, #8998, .T. ) ;
#1575 = CARTESIAN_POINT ( 'NONE',  ( 3.000000000000000888, 22.83456483164692585, -2.745295967525759995 ) ) ;
#1576 = EDGE_LOOP ( 'NONE', ( #4957, #154, #8345, #6343 ) ) ;
#1577 = EDGE_LOOP ( 'NONE', ( #3409, #4019, #9660, #8524 ) ) ;
#1578 =( GEOMETRIC_REPRESENTATION_CONTEXT ( 3 ) GLOBAL_UNCERTAINTY_ASSIGNED_CONTEXT ( ( #2564 ) ) GLOBAL_UNIT_ASSIGNED_CONTEXT ( ( #752, #2712, #4616 ) ) REPRESENTATION_CONTEXT ( 'NONE', 'WORKASPACE' ) );
#1579 = EDGE_CURVE ( 'NONE', #3895, #8886, #10368, .T. ) ;
#1580 = EDGE_LOOP ( 'NONE', ( #3082, #9963, #2261, #1740 ) ) ;
#1581 = CARTESIAN_POINT ( 'NONE',  ( 3.000000000000000888, -15.13242714128107913, -17.31945870441162683 ) ) ;
#1582 = DIRECTION ( 'NONE',  ( 0.000000000000000000, -0.1045284632676401204, -0.9945218953682746221 ) ) ;
#1583 = AXIS2_PLACEMENT_3D ( 'NONE', #2801, #4577, #10132 ) ;
#1584 = PRODUCT_DEFINITION_CONTEXT ( 'detailed design', #11146, 'design' ) ;
#1585 = LINE ( 'NONE', #11913, #7552 ) ;
#1586 = AXIS2_PLACEMENT_3D ( 'NONE', #9346, #40, #3789 ) ;
#1587 = VERTEX_POINT ( 'NONE', #2847 ) ;
#1588 = VECTOR ( 'NONE', #7266, 1000.000000000000000 ) ;
#1589 = DIRECTION ( 'NONE',  ( 0.000000000000000000, 0.9135454576425992013, 0.4067366430758040385 ) ) ;
#1590 = DIRECTION ( 'NONE',  ( 0.000000000000000000, -0.3090169943749543902, 0.9510565162951514218 ) ) ;
#1591 = CARTESIAN_POINT ( 'NONE',  ( 11.51680056346191883, -0.3781118375584790470, 6.857782953271941950E-17 ) ) ;
#1592 = CIRCLE ( 'NONE', #5306, 9.599999999999996092 ) ;
#1593 = DIRECTION ( 'NONE',  ( -1.000000000000000000, -0.000000000000000000, -0.000000000000000000 ) ) ;
#1594 = AXIS2_PLACEMENT_3D ( 'NONE', #9402, #8551, #1028 ) ;
#1595 = FACE_OUTER_BOUND ( 'NONE', #8601, .T. ) ;
#1596 = VECTOR ( 'NONE', #1496, 1000.000000000000000 ) ;
#1597 = ORIENTED_EDGE ( 'NONE', *, *, #3540, .F. ) ;
#1598 = CIRCLE ( 'NONE', #5898, 9.599999999999997868 ) ;
#1599 = EDGE_LOOP ( 'NONE', ( #1380, #11703, #2636, #6901 ) ) ;
#1600 = CARTESIAN_POINT ( 'NONE',  ( -6.925491926712309620, 5.292860106065908177, 10.00000000000000000 ) ) ;
#1601 = EDGE_LOOP ( 'NONE', ( #810, #8925, #10839, #2380 ) ) ;
#1602 = CARTESIAN_POINT ( 'NONE',  ( 3.000000000000000888, -24.77821629063821263, -1.039229259764747004 ) ) ;
#1603 = ORIENTED_EDGE ( 'NONE', *, *, #11072, .T. ) ;
#1604 = CIRCLE ( 'NONE', #6680, 9.599999999999999645 ) ;
#1605 = DIRECTION ( 'NONE',  ( 0.000000000000000000, 0.000000000000000000, 1.000000000000000000 ) ) ;
#1606 = VECTOR ( 'NONE', #11275, 1000.000000000000000 ) ;
#1607 = CARTESIAN_POINT ( 'NONE',  ( 3.000000000000000888, 1.039229259764835600, -24.77821629063820907 ) ) ;
#1608 = CARTESIAN_POINT ( 'NONE',  ( 2.798030692817974341, 8.692477993603725750, 10.00000000000000000 ) ) ;
#1609 = DIRECTION ( 'NONE',  ( 0.000000000000000000, 0.000000000000000000, 1.000000000000000000 ) ) ;
#1610 = ADVANCED_FACE ( 'NONE', ( #7296 ), #2662, .T. ) ;
#1611 = CARTESIAN_POINT ( 'NONE',  ( 3.000000000000000888, -19.75591328264879110, -10.87771529938182091 ) ) ;
#1612 = ORIENTED_EDGE ( 'NONE', *, *, #5481, .T. ) ;
#1613 = DIRECTION ( 'NONE',  ( -1.000000000000000000, 0.000000000000000000, 0.000000000000000000 ) ) ;
#1614 = VECTOR ( 'NONE', #64, 1000.000000000000000 ) ;
#1615 = ORIENTED_EDGE ( 'NONE', *, *, #6080, .F. ) ;
#1616 = AXIS2_PLACEMENT_3D ( 'NONE', #2628, #6184, #542 ) ;
#1617 = CARTESIAN_POINT ( 'NONE',  ( 4.212679447664376298, 6.814025269448777955, 3.747395293195558847E-16 ) ) ;
#1618 = CIRCLE ( 'NONE', #234, 9.599999999999999645 ) ;
#1619 = CARTESIAN_POINT ( 'NONE',  ( 3.000000000000000888, -13.23915371906942440, -18.80635025205183197 ) ) ;
#1620 = ORIENTED_EDGE ( 'NONE', *, *, #5353, .T. ) ;
#1621 = EDGE_CURVE ( 'NONE', #3019, #10826, #10249, .T. ) ;
#1622 = CARTESIAN_POINT ( 'NONE',  ( 0.000000000000000000, 23.05871956130122413, 9.128825345753107001 ) ) ;
#1623 = FACE_OUTER_BOUND ( 'NONE', #2541, .T. ) ;
#1624 = CARTESIAN_POINT ( 'NONE',  ( 5.312937634500610073, -1.259815497212794400, 10.00000000000000000 ) ) ;
#1625 = VECTOR ( 'NONE', #9340, 1000.000000000000000 ) ;
#1626 = CARTESIAN_POINT ( 'NONE',  ( 10.96671743108978525, -3.132869264233209439, 6.857782953271941950E-17 ) ) ;
#1627 = DIRECTION ( 'NONE',  ( 0.000000000000000000, 0.000000000000000000, 1.000000000000000000 ) ) ;
#1628 = LINE ( 'NONE', #6160, #11534 ) ;
#1629 = CIRCLE ( 'NONE', #254, 9.599999999999997868 ) ;
#1630 = VERTEX_POINT ( 'NONE', #1862 ) ;
#1631 = EDGE_LOOP ( 'NONE', ( #9715, #6175, #6162, #10993 ) ) ;
#1632 = CARTESIAN_POINT ( 'NONE',  ( -7.115032382426030644, -13.85544350050026807, 10.00000000000000000 ) ) ;
#1633 = CARTESIAN_POINT ( 'NONE',  ( 0.000000000000000000, 2.745295967525994918, 22.83456483164690098 ) ) ;
#1634 = CIRCLE ( 'NONE', #8485, 9.599999999999999645 ) ;
#1635 = DIRECTION ( 'NONE',  ( 1.000000000000000000, -0.000000000000000000, -0.000000000000000000 ) ) ;
#1636 = CARTESIAN_POINT ( 'NONE',  ( -1.784247137544765716, 5.123456263349895679, 3.747395293195558847E-16 ) ) ;
#1637 = VECTOR ( 'NONE', #6960, 1000.000000000000000 ) ;
#1638 = FACE_OUTER_BOUND ( 'NONE', #10224, .T. ) ;
#1639 = CARTESIAN_POINT ( 'NONE',  ( 3.000000000000000888, 15.64281154287597353, 16.85990652506905363 ) ) ;
#1640 = VERTEX_POINT ( 'NONE', #4561 ) ;
#1641 = APPLICATION_PROTOCOL_DEFINITION ( 'draft international standard', 'automotive_design', 1998, #2788 ) ;
#1642 = ORIENTED_EDGE ( 'NONE', *, *, #4409, .F. ) ;
#1643 = DIRECTION ( 'NONE',  ( -1.000000000000000000, 0.000000000000000000, 0.000000000000000000 ) ) ;
#1644 = EDGE_CURVE ( 'NONE', #4353, #2834, #9779, .T. ) ;
#1645 = DIRECTION ( 'NONE',  ( 1.000000000000000000, 0.000000000000000000, 0.000000000000000000 ) ) ;
#1646 = AXIS2_PLACEMENT_3D ( 'NONE', #1177, #1120, #3877 ) ;
#1647 = DIRECTION ( 'NONE',  ( 0.000000000000000000, 0.000000000000000000, 1.000000000000000000 ) ) ;
#1648 = VERTEX_POINT ( 'NONE', #195 ) ;
#1649 = EDGE_CURVE ( 'NONE', #845, #11767, #5039, .T. ) ;
#1650 = CARTESIAN_POINT ( 'NONE',  ( 3.000000000000000888, -21.30300407174357957, -7.402892494506506438 ) ) ;
#1651 = ADVANCED_FACE ( 'NONE', ( #4059, #6690 ), #2970, .F. ) ;
#1652 = DIRECTION ( 'NONE',  ( 0.000000000000000000, 0.9781476007338049117, 0.2079116908177629230 ) ) ;
#1653 = CARTESIAN_POINT ( 'NONE',  ( -2.061894914253512123, 6.087690860853031793, 6.857782953271941950E-17 ) ) ;
#1654 = CARTESIAN_POINT ( 'NONE',  ( 3.000000000000000888, -7.432877647175354596, 21.76479567747239230 ) ) ;
#1655 = ORIENTED_EDGE ( 'NONE', *, *, #8174, .F. ) ;
#1656 = CARTESIAN_POINT ( 'NONE',  ( 0.000000000000000000, -11.79560690673858403, -19.74380051311552364 ) ) ;
#1657 = VERTEX_POINT ( 'NONE', #10608 ) ;
#1658 = ORIENTED_EDGE ( 'NONE', *, *, #3965, .F. ) ;
#1659 = CARTESIAN_POINT ( 'NONE',  ( -4.491015865170432164, 3.510096388331073403, 10.00000000000000000 ) ) ;
#1660 = ORIENTED_EDGE ( 'NONE', *, *, #8034, .T. ) ;
#1661 = DIRECTION ( 'NONE',  ( 0.000000000000000000, 0.000000000000000000, 1.000000000000000000 ) ) ;
#1662 = ORIENTED_EDGE ( 'NONE', *, *, #12112, .F. ) ;
#1663 = CARTESIAN_POINT ( 'NONE',  ( 3.000000000000000888, -13.72351598154911478, 20.65684170206486669 ) ) ;
#1664 = DIRECTION ( 'NONE',  ( -1.000000000000000000, 0.000000000000000000, -0.000000000000000000 ) ) ;
#1665 = CARTESIAN_POINT ( 'NONE',  ( 3.913389251769919586, -3.458713887698555922, 10.00000000000000000 ) ) ;
#1666 = DIRECTION ( 'NONE',  ( 0.000000000000000000, -0.7431448254773999063, 0.6691306063588519093 ) ) ;
#1667 = CARTESIAN_POINT ( 'NONE',  ( 3.000000000000000888, 22.47229024614977533, 1.901833551798334909 ) ) ;
#1668 = CYLINDRICAL_SURFACE ( 'NONE', #996, 9.599999999999999645 ) ;
#1669 = ORIENTED_EDGE ( 'NONE', *, *, #4258, .F. ) ;
#1670 = EDGE_CURVE ( 'NONE', #6927, #2739, #11924, .T. ) ;
#1671 = VECTOR ( 'NONE', #2711, 1000.000000000000000 ) ;
#1672 = CARTESIAN_POINT ( 'NONE',  ( 1.445324715877976729, -3.701599742324197084, 3.747395293195558847E-16 ) ) ;
#1673 = DIRECTION ( 'NONE',  ( -1.000000000000000000, -0.000000000000000000, -0.000000000000000000 ) ) ;
#1674 = CARTESIAN_POINT ( 'NONE',  ( 0.000000000000000000, 0.000000000000000000, 0.000000000000000000 ) ) ;
#1675 = ORIENTED_EDGE ( 'NONE', *, *, #2091, .F. ) ;
#1676 = ADVANCED_FACE ( 'NONE', ( #8720 ), #2103, .T. ) ;
#1677 = DIRECTION ( 'NONE',  ( 0.000000000000000000, 0.4067366430758009854, -0.9135454576426006446 ) ) ;
#1678 = DIRECTION ( 'NONE',  ( 0.000000000000000000, 0.000000000000000000, 1.000000000000000000 ) ) ;
#1679 = CARTESIAN_POINT ( 'NONE',  ( -1.032305814202113092, 6.265050879046242471, 10.00000000000000000 ) ) ;
#1680 = AXIS2_PLACEMENT_3D ( 'NONE', #5953, #9680, #8767 ) ;
#1681 = CARTESIAN_POINT ( 'NONE',  ( -7.040021908109678428, -0.4595208068204874041, 6.857782953271941950E-17 ) ) ;
#1682 = CARTESIAN_POINT ( 'NONE',  ( -10.00000000000000000, 0.000000000000000000, 0.000000000000000000 ) ) ;
#1683 = CYLINDRICAL_SURFACE ( 'NONE', #7220, 9.599999999999999645 ) ;
#1684 = EDGE_LOOP ( 'NONE', ( #2344, #3840, #4959, #5878 ) ) ;
#1685 = EDGE_CURVE ( 'NONE', #6263, #6662, #11724, .T. ) ;
#1686 = ORIENTED_EDGE ( 'NONE', *, *, #3487, .T. ) ;
#1687 = ORIENTED_EDGE ( 'NONE', *, *, #8757, .T. ) ;
#1688 = VECTOR ( 'NONE', #1404, 1000.000000000000000 ) ;
#1689 = CARTESIAN_POINT ( 'NONE',  ( -14.60057116351880069, -4.165219547604622541, 10.00000000000000000 ) ) ;
#1690 = CYLINDRICAL_SURFACE ( 'NONE', #8580, 22.99899999999999878 ) ;
#1691 = CARTESIAN_POINT ( 'NONE',  ( 0.000000000000000000, 0.000000000000000000, 0.000000000000000000 ) ) ;
#1692 = CARTESIAN_POINT ( 'NONE',  ( -1.790740696106538632, -6.394195405909704810, 3.747395293195558847E-16 ) ) ;
#1693 = CARTESIAN_POINT ( 'NONE',  ( -5.000000000000000000, 0.000000000000000000, 1.000000000000000000 ) ) ;
#1694 = VERTEX_POINT ( 'NONE', #7730 ) ;
#1695 = CIRCLE ( 'NONE', #6958, 22.99899999999999878 ) ;
#1696 = CARTESIAN_POINT ( 'NONE',  ( 0.000000000000000000, -20.08719549084872824, 11.20082935824068038 ) ) ;
#1697 = ORIENTED_EDGE ( 'NONE', *, *, #3079, .F. ) ;
#1698 = EDGE_LOOP ( 'NONE', ( #10381, #4428, #11078, #5847 ) ) ;
#1699 = DIRECTION ( 'NONE',  ( -1.000000000000000000, 0.000000000000000000, 0.000000000000000000 ) ) ;
#1700 = CARTESIAN_POINT ( 'NONE',  ( 3.000000000000000888, -24.45282072769603587, 4.135161237383499611 ) ) ;
#1701 = DIRECTION ( 'NONE',  ( 0.000000000000000000, -0.9510565162951565288, 0.3090169943749382364 ) ) ;
#1702 = DIRECTION ( 'NONE',  ( -1.000000000000000000, -0.000000000000000000, -0.000000000000000000 ) ) ;
#1703 = DIRECTION ( 'NONE',  ( 0.000000000000000000, 0.9945218953682729568, 0.1045284632676570929 ) ) ;
#1704 = CARTESIAN_POINT ( 'NONE',  ( 0.000000000000000000, -22.54798042742717357, 9.142421143074578538 ) ) ;
#1705 = DIRECTION ( 'NONE',  ( 0.000000000000000000, 0.8660254037844400399, -0.4999999999999978906 ) ) ;
#1706 = VERTEX_POINT ( 'NONE', #3088 ) ;
#1707 = CARTESIAN_POINT ( 'NONE',  ( 1.500000000000000444, 21.97817939804039611, 11.48910920600691732 ) ) ;
#1708 = ORIENTED_EDGE ( 'NONE', *, *, #5083, .T. ) ;
#1709 = AXIS2_PLACEMENT_3D ( 'NONE', #8770, #375, #10664 ) ;
#1710 = ORIENTED_EDGE ( 'NONE', *, *, #8972, .F. ) ;
#1711 = CARTESIAN_POINT ( 'NONE',  ( 7.402789038520873000, -0.9464297003978345835, 10.00000000000000000 ) ) ;
#1712 = EDGE_CURVE ( 'NONE', #2147, #4846, #5476, .T. ) ;
#1713 = DIRECTION ( 'NONE',  ( -1.000000000000000000, -0.000000000000000000, 0.000000000000000000 ) ) ;
#1714 = ORIENTED_EDGE ( 'NONE', *, *, #10084, .T. ) ;
#1715 = EDGE_CURVE ( 'NONE', #8966, #1364, #9588, .T. ) ;
#1716 = DIRECTION ( 'NONE',  ( 0.000000000000000000, -0.7431448254773999063, 0.6691306063588519093 ) ) ;
#1717 = DIRECTION ( 'NONE',  ( -1.000000000000000000, -0.000000000000000000, -0.000000000000000000 ) ) ;
#1718 = CARTESIAN_POINT ( 'NONE',  ( 4.382127860174850120, -16.35473703246190524, 6.857782953271941950E-17 ) ) ;
#1719 = AXIS2_PLACEMENT_3D ( 'NONE', #5033, #6010, #5893 ) ;
#1720 = CARTESIAN_POINT ( 'NONE',  ( 0.000000000000000000, -20.41249101028218149, 9.589108953447823325 ) ) ;
#1721 = VERTEX_POINT ( 'NONE', #135 ) ;
#1722 = DIRECTION ( 'NONE',  ( 0.000000000000000000, 0.9510565162951543083, -0.3090169943749450643 ) ) ;
#1723 = EDGE_LOOP ( 'NONE', ( #5800, #6317, #4097, #7504 ) ) ;
#1724 = EDGE_CURVE ( 'NONE', #9035, #12008, #3917, .T. ) ;
#1725 = CARTESIAN_POINT ( 'NONE',  ( 7.357672848543031385, 2.125097602832226151, 3.747395293195558847E-16 ) ) ;
#1726 = VECTOR ( 'NONE', #5002, 1000.000000000000000 ) ;
#1727 = CARTESIAN_POINT ( 'NONE',  ( 3.000000000000000888, -2.811977935937640005, -22.37663021667346896 ) ) ;
#1728 = CARTESIAN_POINT ( 'NONE',  ( 0.000000000000000000, 6.668524164681629784, 23.88662356770117512 ) ) ;
#1729 = CYLINDRICAL_SURFACE ( 'NONE', #9021, 9.599999999999997868 ) ;
#1730 = DIRECTION ( 'NONE',  ( 0.000000000000000000, 0.5877852522924741363, -0.8090169943749467851 ) ) ;
#1731 = DIRECTION ( 'NONE',  ( -1.000000000000000000, 0.000000000000000000, -0.000000000000000000 ) ) ;
#1732 = ADVANCED_FACE ( 'NONE', ( #9631 ), #263, .T. ) ;
#1733 = CARTESIAN_POINT ( 'NONE',  ( -3.542987847618818353, 5.503081486278154522, 6.857782953271941950E-17 ) ) ;
#1734 = CARTESIAN_POINT ( 'NONE',  ( 0.000000000000000000, 0.000000000000000000, 0.000000000000000000 ) ) ;
#1735 = CIRCLE ( 'NONE', #2120, 4.000000000000000000 ) ;
#1736 = DIRECTION ( 'NONE',  ( 0.000000000000000000, 0.000000000000000000, 1.000000000000000000 ) ) ;
#1737 = ORIENTED_EDGE ( 'NONE', *, *, #3104, .F. ) ;
#1738 = EDGE_CURVE ( 'NONE', #5993, #4594, #9452, .T. ) ;
#1739 = VERTEX_POINT ( 'NONE', #9689 ) ;
#1740 = ORIENTED_EDGE ( 'NONE', *, *, #3104, .T. ) ;
#1741 = PLANE ( 'NONE',  #6816 ) ;
#1742 = CARTESIAN_POINT ( 'NONE',  ( -11.32214898804313208, 3.633524203737720448, 10.00000000000000000 ) ) ;
#1743 = CARTESIAN_POINT ( 'NONE',  ( -19.00000000000000000, 2.326828918379970970E-15, -5.000000000000000000 ) ) ;
#1744 = CARTESIAN_POINT ( 'NONE',  ( 0.000000000000000000, 0.000000000000000000, -15.00000000000000000 ) ) ;
#1745 = AXIS2_PLACEMENT_3D ( 'NONE', #8867, #1394, #470 ) ;
#1746 = CARTESIAN_POINT ( 'NONE',  ( -0.3758430365714711674, 11.29677535215814110, 3.747395293195558847E-16 ) ) ;
#1747 = LINE ( 'NONE', #11244, #3378 ) ;
#1748 = CARTESIAN_POINT ( 'NONE',  ( 0.000000000000000000, 0.000000000000000000, -15.00000000000000000 ) ) ;
#1749 = CARTESIAN_POINT ( 'NONE',  ( 1.499999999999999556, -6.668524164681792321, 23.88662356770113249 ) ) ;
#1750 = ADVANCED_FACE ( 'NONE', ( #6806 ), #4985, .T. ) ;
#1751 = VERTEX_POINT ( 'NONE', #3947 ) ;
#1752 = VERTEX_POINT ( 'NONE', #1304 ) ;
#1753 = AXIS2_PLACEMENT_3D ( 'NONE', #8898, #6983, #1486 ) ;
#1754 = ORIENTED_EDGE ( 'NONE', *, *, #2693, .F. ) ;
#1755 = DIRECTION ( 'NONE',  ( 0.000000000000000000, 0.000000000000000000, 1.000000000000000000 ) ) ;
#1756 = CARTESIAN_POINT ( 'NONE',  ( 1.500000000000000444, -21.97817939804047427, 11.48910920600676278 ) ) ;
#1757 = DIRECTION ( 'NONE',  ( -0.000000000000000000, -0.000000000000000000, -1.000000000000000000 ) ) ;
#1758 = CYLINDRICAL_SURFACE ( 'NONE', #5639, 22.99899999999999878 ) ;
#1759 = ADVANCED_FACE ( 'NONE', ( #5901 ), #4004, .F. ) ;
#1760 = AXIS2_PLACEMENT_3D ( 'NONE', #9269, #3584, #4744 ) ;
#1761 = CARTESIAN_POINT ( 'NONE',  ( 5.000000000000000000, 6.123233995736766282E-16, 1.000000000000000000 ) ) ;
#1762 = CIRCLE ( 'NONE', #4121, 9.599999999999996092 ) ;
#1763 = CARTESIAN_POINT ( 'NONE',  ( -12.61273389267802436, -8.731886703669292871, 3.747395293195558847E-16 ) ) ;
#1764 = CARTESIAN_POINT ( 'NONE',  ( 6.242895496888662521, -5.302832405932363713, 6.857782953271941950E-17 ) ) ;
#1765 = PRESENTATION_LAYER_ASSIGNMENT (  '', '', ( #4124 ) ) ;
#1766 = DIRECTION ( 'NONE',  ( -1.000000000000000000, 0.000000000000000000, -0.000000000000000000 ) ) ;
#1767 = ORIENTED_EDGE ( 'NONE', *, *, #10478, .T. ) ;
#1768 = VERTEX_POINT ( 'NONE', #10670 ) ;
#1769 = CARTESIAN_POINT ( 'NONE',  ( -3.500000000000000000, 4.286263797015736595E-16, 1.000000000000000888 ) ) ;
#1770 = CIRCLE ( 'NONE', #10376, 9.599999999999997868 ) ;
#1771 = ORIENTED_EDGE ( 'NONE', *, *, #1917, .F. ) ;
#1772 = ORIENTED_EDGE ( 'NONE', *, *, #2240, .F. ) ;
#1773 = CARTESIAN_POINT ( 'NONE',  ( -6.036922680726761747, -0.4347383792561346771, 10.00000000000000000 ) ) ;
#1774 = AXIS2_PLACEMENT_3D ( 'NONE', #10838, #8885, #1412 ) ;
#1775 = CARTESIAN_POINT ( 'NONE',  ( 3.000000000000000888, 0.000000000000000000, 0.000000000000000000 ) ) ;
#1776 = ORIENTED_EDGE ( 'NONE', *, *, #1341, .F. ) ;
#1777 = DIRECTION ( 'NONE',  ( -1.000000000000000000, 0.000000000000000000, 0.000000000000000000 ) ) ;
#1778 = CARTESIAN_POINT ( 'NONE',  ( 3.000000000000000888, 0.000000000000000000, 0.000000000000000000 ) ) ;
#1779 = CARTESIAN_POINT ( 'NONE',  ( 0.0002901587068752367257, -4.749354241797645315, 10.00000000000000000 ) ) ;
#1780 = AXIS2_PLACEMENT_3D ( 'NONE', #8730, #10620, #390 ) ;
#1781 = CIRCLE ( 'NONE', #4917, 19.99999999999999645 ) ;
#1782 = CARTESIAN_POINT ( 'NONE',  ( 3.000000000000000888, 0.000000000000000000, 0.000000000000000000 ) ) ;
#1783 = VECTOR ( 'NONE', #9935, 1000.000000000000000 ) ;
#1784 = AXIS2_PLACEMENT_3D ( 'NONE', #280, #5923, #2119 ) ;
#1785 = CARTESIAN_POINT ( 'NONE',  ( 0.000000000000000000, 0.000000000000000000, 0.000000000000000000 ) ) ;
#1786 = ORIENTED_EDGE ( 'NONE', *, *, #11985, .T. ) ;
#1787 = ADVANCED_FACE ( 'NONE', ( #7671 ), #2283, .F. ) ;
#1788 = DIRECTION ( 'NONE',  ( -1.000000000000000000, 0.000000000000000000, -0.000000000000000000 ) ) ;
#1789 = ORIENTED_EDGE ( 'NONE', *, *, #6258, .T. ) ;
#1790 = CARTESIAN_POINT ( 'NONE',  ( 4.623190192904133689, -5.402202315098909580, 3.747395293195558847E-16 ) ) ;
#1791 = EDGE_CURVE ( 'NONE', #10729, #10168, #4304, .T. ) ;
#1792 = DIRECTION ( 'NONE',  ( -1.000000000000000000, -0.000000000000000000, -0.000000000000000000 ) ) ;
#1793 = AXIS2_PLACEMENT_3D ( 'NONE', #1469, #8995, #9792 ) ;
#1794 = DIRECTION ( 'NONE',  ( 0.000000000000000000, 0.000000000000000000, 1.000000000000000000 ) ) ;
#1795 = LINE ( 'NONE', #6271, #11992 ) ;
#1796 = CARTESIAN_POINT ( 'NONE',  ( 16.47843063274657993, -5.593696103119286001, 10.00000000000000000 ) ) ;
#1797 = EDGE_CURVE ( 'NONE', #5220, #2390, #6079, .T. ) ;
#1798 = CARTESIAN_POINT ( 'NONE',  ( 8.527474615971319949, 0.9793716136081375145, 6.857782953271941950E-17 ) ) ;
#1799 = CARTESIAN_POINT ( 'NONE',  ( 0.000000000000000000, 0.000000000000000000, 0.000000000000000000 ) ) ;
#1800 = EDGE_CURVE ( 'NONE', #4256, #411, #6650, .T. ) ;
#1801 = VECTOR ( 'NONE', #10905, 1000.000000000000000 ) ;
#1802 = FACE_OUTER_BOUND ( 'NONE', #604, .T. ) ;
#1803 = VECTOR ( 'NONE', #243, 1000.000000000000000 ) ;
#1804 = VERTEX_POINT ( 'NONE', #6200 ) ;
#1805 = ADVANCED_FACE ( 'NONE', ( #11823 ), #10906, .T. ) ;
#1806 = VECTOR ( 'NONE', #4300, 1000.000000000000000 ) ;
#1807 = ORIENTED_EDGE ( 'NONE', *, *, #8560, .T. ) ;
#1808 = CARTESIAN_POINT ( 'NONE',  ( 3.000000000000000888, 18.80635025205187816, -13.23915371906935867 ) ) ;
#1809 = CARTESIAN_POINT ( 'NONE',  ( 9.640149279600557009, 4.768118462334745011, 10.00000000000000000 ) ) ;
#1810 = DIRECTION ( 'NONE',  ( -1.000000000000000000, 0.000000000000000000, -0.000000000000000000 ) ) ;
#1811 =( GEOMETRIC_REPRESENTATION_CONTEXT ( 3 ) GLOBAL_UNCERTAINTY_ASSIGNED_CONTEXT ( ( #478 ) ) GLOBAL_UNIT_ASSIGNED_CONTEXT ( ( #5286, #9878, #2599 ) ) REPRESENTATION_CONTEXT ( 'NONE', 'WORKASPACE' ) );
#1812 = FACE_BOUND ( 'NONE', #10883, .T. ) ;
#1813 = LINE ( 'NONE', #29, #6233 ) ;
#1814 = CARTESIAN_POINT ( 'NONE',  ( -7.370305768634978882, 4.727533884956530486, 3.747395293195558847E-16 ) ) ;
#1815 = DIRECTION ( 'NONE',  ( -1.000000000000000000, 0.000000000000000000, -0.000000000000000000 ) ) ;
#1816 = CARTESIAN_POINT ( 'NONE',  ( 1.499999999999999556, 9.128825345753025289, 23.05871956130125611 ) ) ;
#1817 = ORIENTED_EDGE ( 'NONE', *, *, #4224, .F. ) ;
#1818 = AXIS2_PLACEMENT_3D ( 'NONE', #4837, #7582, #2884 ) ;
#1819 = ORIENTED_EDGE ( 'NONE', *, *, #4948, .T. ) ;
#1820 = ORIENTED_EDGE ( 'NONE', *, *, #10170, .T. ) ;
#1821 = LINE ( 'NONE', #5560, #2215 ) ;
#1822 = AXIS2_PLACEMENT_3D ( 'NONE', #3542, #5380, #3360 ) ;
#1823 = VECTOR ( 'NONE', #2939, 1000.000000000000000 ) ;
#1824 = CARTESIAN_POINT ( 'NONE',  ( 3.000000000000000888, 0.000000000000000000, 0.000000000000000000 ) ) ;
#1825 =( NAMED_UNIT ( * ) PLANE_ANGLE_UNIT ( ) SI_UNIT ( $, .RADIAN. ) );
#1826 = UNCERTAINTY_MEASURE_WITH_UNIT (LENGTH_MEASURE( 1.000000000000000082E-05 ), #3721, 'distance_accuracy_value', 'NONE');
#1827 = FACE_OUTER_BOUND ( 'NONE', #3222, .T. ) ;
#1828 = EDGE_CURVE ( 'NONE', #4090, #1430, #9987, .T. ) ;
#1829 = CYLINDRICAL_SURFACE ( 'NONE', #3983, 22.99899999999999878 ) ;
#1830 = CARTESIAN_POINT ( 'NONE',  ( 13.24268851590353790, -2.403973981684889072, 3.747395293195558847E-16 ) ) ;
#1831 = CARTESIAN_POINT ( 'NONE',  ( 5.312937634499088624, -1.259815497212412261, 6.857782953271941950E-17 ) ) ;
#1832 = DIRECTION ( 'NONE',  ( -1.000000000000000000, -0.000000000000000000, -0.000000000000000000 ) ) ;
#1833 = VERTEX_POINT ( 'NONE', #9925 ) ;
#1834 = ORIENTED_EDGE ( 'NONE', *, *, #1494, .T. ) ;
#1835 = DIRECTION ( 'NONE',  ( 0.000000000000000000, 0.000000000000000000, -1.000000000000000000 ) ) ;
#1836 = EDGE_CURVE ( 'NONE', #7635, #8246, #9077, .T. ) ;
#1837 = ORIENTED_EDGE ( 'NONE', *, *, #5702, .T. ) ;
#1838 = AXIS2_PLACEMENT_3D ( 'NONE', #7608, #1076, #11240 ) ;
#1839 = AXIS2_PLACEMENT_3D ( 'NONE', #10180, #12015, #7172 ) ;
#1840 = ORIENTED_EDGE ( 'NONE', *, *, #11141, .T. ) ;
#1841 = CARTESIAN_POINT ( 'NONE',  ( 3.571029491936648093, 3.388293644658559423, 10.00000000000000000 ) ) ;
#1842 = DIRECTION ( 'NONE',  ( -1.000000000000000000, 0.000000000000000000, 0.000000000000000000 ) ) ;
#1843 = ORIENTED_EDGE ( 'NONE', *, *, #3009, .T. ) ;
#1844 = CARTESIAN_POINT ( 'NONE',  ( -4.500000000000000888, 3.903127820947816751E-15, 3.000000000000000000 ) ) ;
#1845 = DIRECTION ( 'NONE',  ( 0.000000000000000000, 0.000000000000000000, -1.000000000000000000 ) ) ;
#1846 = CARTESIAN_POINT ( 'NONE',  ( -2.682496113117368797, -7.114254743909099510, 10.00000000000000000 ) ) ;
#1847 = CIRCLE ( 'NONE', #6534, 9.599999999999997868 ) ;
#1848 = CARTESIAN_POINT ( 'NONE',  ( 3.000000000000000888, -20.08719549084872824, 11.20082935824068038 ) ) ;
#1849 = DIRECTION ( 'NONE',  ( 0.000000000000000000, 0.3090169943749415671, 0.9510565162951555296 ) ) ;
#1850 = DIRECTION ( 'NONE',  ( -1.000000000000000000, -0.000000000000000000, -0.000000000000000000 ) ) ;
#1851 = VERTEX_POINT ( 'NONE', #11700 ) ;
#1852 = EDGE_LOOP ( 'NONE', ( #10136, #1603, #7225, #5129 ) ) ;
#1853 = CARTESIAN_POINT ( 'NONE',  ( 3.000000000000000888, 7.402892494506291499, 21.30300407174365063 ) ) ;
#1854 = ORIENTED_EDGE ( 'NONE', *, *, #10659, .F. ) ;
#1855 = CARTESIAN_POINT ( 'NONE',  ( 4.140589500486089314, -5.731468560950439439, 3.747395293195558847E-16 ) ) ;
#1856 = AXIS2_PLACEMENT_3D ( 'NONE', #1538, #1904, #11391 ) ;
#1857 = CARTESIAN_POINT ( 'NONE',  ( 3.500000000000000000, 0.000000000000000000, 10.00000000000000000 ) ) ;
#1858 = DIRECTION ( 'NONE',  ( -1.000000000000000000, 0.000000000000000000, 0.000000000000000000 ) ) ;
#1859 = LINE ( 'NONE', #2901, #11618 ) ;
#1860 = CARTESIAN_POINT ( 'NONE',  ( 3.000000000000000000, 0.000000000000000000, 0.000000000000000000 ) ) ;
#1861 = CARTESIAN_POINT ( 'NONE',  ( 4.698850784960272087, -6.565226861933591174, 6.857782953271941950E-17 ) ) ;
#1862 = CARTESIAN_POINT ( 'NONE',  ( 0.000000000000000000, -15.64281154287585807, -16.85990652506916021 ) ) ;
#1863 = ORIENTED_EDGE ( 'NONE', *, *, #2587, .T. ) ;
#1864 = VERTEX_POINT ( 'NONE', #9873 ) ;
#1865 = EDGE_CURVE ( 'NONE', #4536, #2001, #7627, .T. ) ;
#1866 = CARTESIAN_POINT ( 'NONE',  ( 1.500000000000000444, -20.65684170206500170, 13.72351598154890873 ) ) ;
#1867 = CARTESIAN_POINT ( 'NONE',  ( -3.937910939466569005, -8.732312745279401156, 10.00000000000000000 ) ) ;
#1868 = ADVANCED_FACE ( 'NONE', ( #5219 ), #8152, .T. ) ;
#1869 = CARTESIAN_POINT ( 'NONE',  ( 1.499999999999999556, 22.21333432029578603, -11.02759168516723065 ) ) ;
#1870 = CARTESIAN_POINT ( 'NONE',  ( 3.000000000000000888, -15.13242714128107913, -17.31945870441162683 ) ) ;
#1871 = DIRECTION ( 'NONE',  ( 0.000000000000000000, 0.000000000000000000, 1.000000000000000000 ) ) ;
#1872 = AXIS2_PLACEMENT_3D ( 'NONE', #1310, #9877, #6152 ) ;
#1873 = EDGE_CURVE ( 'NONE', #9943, #8329, #2159, .T. ) ;
#1874 = ADVANCED_FACE ( 'NONE', ( #5347 ), #5159, .T. ) ;
#1875 = CARTESIAN_POINT ( 'NONE',  ( 6.685168693379560878, -7.607270790100919555, 3.747395293195558847E-16 ) ) ;
#1876 = CARTESIAN_POINT ( 'NONE',  ( 3.000000000000000888, -21.30300407174367905, 7.402892494506218668 ) ) ;
#1877 = CARTESIAN_POINT ( 'NONE',  ( 1.499999999999999556, 23.88662356770124262, -6.668524164681381095 ) ) ;
#1878 = ORIENTED_EDGE ( 'NONE', *, *, #2996, .T. ) ;
#1879 = ORIENTED_EDGE ( 'NONE', *, *, #10996, .T. ) ;
#1880 = ORIENTED_EDGE ( 'NONE', *, *, #10259, .T. ) ;
#1881 = VERTEX_POINT ( 'NONE', #1362 ) ;
#1882 = EDGE_CURVE ( 'NONE', #4541, #3273, #3926, .T. ) ;
#1883 = DIRECTION ( 'NONE',  ( 0.000000000000000000, 0.3090169943749479509, -0.9510565162951534202 ) ) ;
#1884 = CYLINDRICAL_SURFACE ( 'NONE', #10765, 9.599999999999997868 ) ;
#1885 = DIRECTION ( 'NONE',  ( 0.000000000000000000, 0.000000000000000000, -1.000000000000000000 ) ) ;
#1886 = CARTESIAN_POINT ( 'NONE',  ( 3.000000000000000888, 22.47229024614980020, -1.901833551798019162 ) ) ;
#1887 = DIRECTION ( 'NONE',  ( 1.000000000000000000, 0.000000000000000000, 0.000000000000000000 ) ) ;
#1888 = VECTOR ( 'NONE', #9428, 1000.000000000000000 ) ;
#1889 = CARTESIAN_POINT ( 'NONE',  ( 11.62709622633471618, -6.461356448465071622, 3.747395293195558847E-16 ) ) ;
#1890 = CARTESIAN_POINT ( 'NONE',  ( -2.100379401128184664, -7.348625593045285065, 6.857782953271941950E-17 ) ) ;
#1891 = ADVANCED_FACE ( 'NONE', ( #4240 ), #1543, .T. ) ;
#1892 = DIRECTION ( 'NONE',  ( 0.000000000000000000, 0.000000000000000000, 1.000000000000000000 ) ) ;
#1893 = ORIENTED_EDGE ( 'NONE', *, *, #10184, .T. ) ;
#1894 = ORIENTED_EDGE ( 'NONE', *, *, #8228, .T. ) ;
#1895 = DIRECTION ( 'NONE',  ( 0.000000000000000000, 0.000000000000000000, 1.000000000000000000 ) ) ;
#1896 = VERTEX_POINT ( 'NONE', #3508 ) ;
#1897 = ADVANCED_FACE ( 'NONE', ( #4185 ), #6017, .T. ) ;
#1898 = ORIENTED_EDGE ( 'NONE', *, *, #7307, .F. ) ;
#1899 = CARTESIAN_POINT ( 'NONE',  ( 3.000000000000000888, 0.000000000000000000, 0.000000000000000000 ) ) ;
#1900 = FACE_OUTER_BOUND ( 'NONE', #10052, .T. ) ;
#1901 = EDGE_LOOP ( 'NONE', ( #10810, #447, #290, #2117 ) ) ;
#1902 = DIRECTION ( 'NONE',  ( -1.000000000000000000, 0.000000000000000000, -0.000000000000000000 ) ) ;
#1903 = EDGE_CURVE ( 'NONE', #1167, #6070, #1966, .T. ) ;
#1904 = DIRECTION ( 'NONE',  ( -1.000000000000000000, -0.000000000000000000, 0.000000000000000000 ) ) ;
#1905 = CARTESIAN_POINT ( 'NONE',  ( -6.829322889802586616, -2.192323464439263514, 10.00000000000000000 ) ) ;
#1906 = DIRECTION ( 'NONE',  ( 1.000000000000000000, 0.000000000000000000, 0.000000000000000000 ) ) ;
#1907 = CARTESIAN_POINT ( 'NONE',  ( 0.000000000000000000, -4.135161237383401911, -24.45282072769605364 ) ) ;
#1908 = AXIS2_PLACEMENT_3D ( 'NONE', #3517, #10863, #1677 ) ;
#1909 = DIRECTION ( 'NONE',  ( -1.000000000000000000, -0.000000000000000000, 0.000000000000000000 ) ) ;
#1910 = VERTEX_POINT ( 'NONE', #7912 ) ;
#1911 = CARTESIAN_POINT ( 'NONE',  ( -2.958039891549808953, -0.4999999999999997780, 3.000000000000000000 ) ) ;
#1912 = VERTEX_POINT ( 'NONE', #3321 ) ;
#1913 = CARTESIAN_POINT ( 'NONE',  ( -13.83044629298881389, 5.462350471645223138, 10.00000000000000000 ) ) ;
#1914 = CARTESIAN_POINT ( 'NONE',  ( 3.000000000000000888, -22.37663021667346186, 2.811977935937707063 ) ) ;
#1915 = AXIS2_PLACEMENT_3D ( 'NONE', #4053, #11517, #11693 ) ;
#1916 = DIRECTION ( 'NONE',  ( -1.000000000000000000, -0.000000000000000000, -0.000000000000000000 ) ) ;
#1917 = EDGE_CURVE ( 'NONE', #862, #7927, #2364, .T. ) ;
#1918 = CARTESIAN_POINT ( 'NONE',  ( 3.000000000000000888, -9.667200211209964422, 20.86861857134731579 ) ) ;
#1919 = CARTESIAN_POINT ( 'NONE',  ( -3.791520748785662587, -16.26028641251513207, 10.00000000000000000 ) ) ;
#1920 = CARTESIAN_POINT ( 'NONE',  ( -5.542557460684657045, -4.854674288179716690, 6.857782953271941950E-17 ) ) ;
#1921 = CARTESIAN_POINT ( 'NONE',  ( 0.000000000000000000, 18.40266524480588473, 13.79477846460802226 ) ) ;
#1922 = DIRECTION ( 'NONE',  ( -1.000000000000000000, 0.000000000000000000, 0.000000000000000000 ) ) ;
#1923 = ORIENTED_EDGE ( 'NONE', *, *, #5774, .T. ) ;
#1924 = AXIS2_PLACEMENT_3D ( 'NONE', #343, #5983, #9767 ) ;
#1925 = VECTOR ( 'NONE', #3531, 1000.000000000000000 ) ;
#1926 = ORIENTED_EDGE ( 'NONE', *, *, #5951, .F. ) ;
#1927 = CYLINDRICAL_SURFACE ( 'NONE', #5822, 24.80000000000000071 ) ;
#1928 = CARTESIAN_POINT ( 'NONE',  ( 4.889075487038677004, 9.929493272051477248, 10.00000000000000000 ) ) ;
#1929 = DIRECTION ( 'NONE',  ( -1.000000000000000000, -0.000000000000000000, -0.000000000000000000 ) ) ;
#1930 = CARTESIAN_POINT ( 'NONE',  ( -5.773631947676829412, 9.989728373610901713, 3.747395293195558847E-16 ) ) ;
#1931 = AXIS2_PLACEMENT_3D ( 'NONE', #9338, #8429, #3711 ) ;
#1932 = AXIS2_PLACEMENT_3D ( 'NONE', #6931, #3095, #6814 ) ;
#1933 = CARTESIAN_POINT ( 'NONE',  ( 3.571029491936644540, 3.388293644658557646, 3.747395293195558847E-16 ) ) ;
#1934 = DIRECTION ( 'NONE',  ( -1.000000000000000000, 0.000000000000000000, 0.000000000000000000 ) ) ;
#1935 = ORIENTED_EDGE ( 'NONE', *, *, #72, .F. ) ;
#1936 = VERTEX_POINT ( 'NONE', #6982 ) ;
#1937 = ORIENTED_EDGE ( 'NONE', *, *, #6948, .F. ) ;
#1938 = EDGE_CURVE ( 'NONE', #401, #1454, #7836, .T. ) ;
#1939 = ORIENTED_EDGE ( 'NONE', *, *, #3598, .T. ) ;
#1940 = DIRECTION ( 'NONE',  ( 0.000000000000000000, 0.000000000000000000, 1.000000000000000000 ) ) ;
#1941 = AXIS2_PLACEMENT_3D ( 'NONE', #850, #11123, #2811 ) ;
#1942 = DIRECTION ( 'NONE',  ( 1.000000000000000000, 0.000000000000000000, 0.000000000000000000 ) ) ;
#1943 = EDGE_CURVE ( 'NONE', #6070, #10397, #9210, .T. ) ;
#1944 = CYLINDRICAL_SURFACE ( 'NONE', #12102, 9.599999999999997868 ) ;
#1945 = FACE_OUTER_BOUND ( 'NONE', #10754, .T. ) ;
#1946 = DIRECTION ( 'NONE',  ( -1.000000000000000000, -0.000000000000000000, 0.000000000000000000 ) ) ;
#1947 = CARTESIAN_POINT ( 'NONE',  ( 5.172292865810426576, -11.91455349003027564, 3.747395293195558847E-16 ) ) ;
#1948 = CARTESIAN_POINT ( 'NONE',  ( 0.000000000000000000, 0.000000000000000000, 0.000000000000000000 ) ) ;
#1949 = ADVANCED_FACE ( 'NONE', ( #9315 ), #9130, .T. ) ;
#1950 = EDGE_CURVE ( 'NONE', #5661, #11556, #1770, .T. ) ;
#1951 = LINE ( 'NONE', #11378, #8221 ) ;
#1952 = ORIENTED_EDGE ( 'NONE', *, *, #5226, .F. ) ;
#1953 = ORIENTED_EDGE ( 'NONE', *, *, #7931, .F. ) ;
#1954 = CARTESIAN_POINT ( 'NONE',  ( -7.575117642440520882, -14.74712341115847103, 10.00000000000000000 ) ) ;
#1955 = ORIENTED_EDGE ( 'NONE', *, *, #1574, .T. ) ;
#1956 = CARTESIAN_POINT ( 'NONE',  ( 0.000000000000000000, 7.432877647175492264, -21.76479567747234256 ) ) ;
#1957 = VECTOR ( 'NONE', #8675, 1000.000000000000000 ) ;
#1958 = LINE ( 'NONE', #5700, #1888 ) ;
#1959 = VERTEX_POINT ( 'NONE', #4476 ) ;
#1960 = AXIS2_PLACEMENT_3D ( 'NONE', #10366, #10075, #8245 ) ;
#1961 = DIRECTION ( 'NONE',  ( -0.000000000000000000, -0.000000000000000000, -1.000000000000000000 ) ) ;
#1962 = FACE_OUTER_BOUND ( 'NONE', #472, .T. ) ;
#1963 = CARTESIAN_POINT ( 'NONE',  ( 14.22875512193218661, -2.589574901423981057, 6.857782953271941950E-17 ) ) ;
#1964 = EDGE_CURVE ( 'NONE', #1098, #9240, #601, .T. ) ;
#1965 = LINE ( 'NONE', #1108, #1614 ) ;
#1966 = CIRCLE ( 'NONE', #804, 9.599999999999996092 ) ;
#1967 = DIRECTION ( 'NONE',  ( 0.000000000000000000, -0.8090169943749407899, -0.5877852522924824630 ) ) ;
#1968 = ORIENTED_EDGE ( 'NONE', *, *, #9908, .F. ) ;
#1969 = ORIENTED_EDGE ( 'NONE', *, *, #1273, .T. ) ;
#1970 = CARTESIAN_POINT ( 'NONE',  ( 3.000000000000000888, 22.54798042742718067, 9.142421143074731305 ) ) ;
#1971 = VECTOR ( 'NONE', #5712, 1000.000000000000000 ) ;
#1972 = VERTEX_POINT ( 'NONE', #7406 ) ;
#1973 = CARTESIAN_POINT ( 'NONE',  ( -8.499083411061075566, 11.86528080735166490, 10.00000000000000000 ) ) ;
#1974 = DIRECTION ( 'NONE',  ( 0.000000000000000000, -0.5000000000000072164, 0.8660254037844344888 ) ) ;
#1975 = SURFACE_SIDE_STYLE ('',( #9262 ) ) ;
#1976 = ORIENTED_EDGE ( 'NONE', *, *, #8938, .F. ) ;
#1977 = AXIS2_PLACEMENT_3D ( 'NONE', #12060, #5523, #3627 ) ;
#1979 = VECTOR ( 'NONE', #12029, 1000.000000000000000 ) ;
#1978 = LINE ( 'NONE', #1176, #2690 ) ;
#1980 = DIRECTION ( 'NONE',  ( -1.000000000000000000, 0.000000000000000000, 0.000000000000000000 ) ) ;
#1981 = DIRECTION ( 'NONE',  ( 0.000000000000000000, 0.000000000000000000, 1.000000000000000000 ) ) ;
#1982 = EDGE_CURVE ( 'NONE', #11898, #12091, #9401, .T. ) ;
#1983 = CYLINDRICAL_SURFACE ( 'NONE', #4542, 22.99899999999999878 ) ;
#1984 = CARTESIAN_POINT ( 'NONE',  ( 3.000000000000000888, 0.000000000000000000, 0.000000000000000000 ) ) ;
#1985 = DIRECTION ( 'NONE',  ( -1.000000000000000000, -0.000000000000000000, 0.000000000000000000 ) ) ;
#1986 = DIRECTION ( 'NONE',  ( 0.000000000000000000, -0.9781476007338079093, 0.2079116908177492118 ) ) ;
#1987 = AXIS2_PLACEMENT_3D ( 'NONE', #5912, #3331, #8784 ) ;
#1988 = VECTOR ( 'NONE', #4940, 1000.000000000000000 ) ;
#1989 = EDGE_CURVE ( 'NONE', #10458, #1768, #9984, .T. ) ;
#1990 = AXIS2_PLACEMENT_3D ( 'NONE', #9826, #9644, #11479 ) ;
#1991 = ORIENTED_EDGE ( 'NONE', *, *, #8419, .T. ) ;
#1992 = DIRECTION ( 'NONE',  ( -1.000000000000000000, 0.000000000000000000, 0.000000000000000000 ) ) ;
#1993 = CARTESIAN_POINT ( 'NONE',  ( -0.3758430365714709454, 11.29677535215814466, 10.00000000000000000 ) ) ;
#1994 = DIRECTION ( 'NONE',  ( 1.000000000000000000, -0.000000000000000000, -0.000000000000000000 ) ) ;
#1995 = COLOUR_RGB ( '', 0.09019608, 0.27058824, 0.51372549) ;
#1996 = CARTESIAN_POINT ( 'NONE',  ( 7.316052646047088714, -7.060001943526879487, 3.747395293195558847E-16 ) ) ;
#1997 = CARTESIAN_POINT ( 'NONE',  ( -12.59589084681760518, 2.937805917057593863, 6.857782953271941950E-17 ) ) ;
#1998 = FACE_OUTER_BOUND ( 'NONE', #612, .T. ) ;
#1999 = ORIENTED_EDGE ( 'NONE', *, *, #12034, .F. ) ;
#2000 = ORIENTED_EDGE ( 'NONE', *, *, #10571, .T. ) ;
#2001 = VERTEX_POINT ( 'NONE', #1907 ) ;
#2002 = DIRECTION ( 'NONE',  ( 1.000000000000000000, -0.000000000000000000, -0.000000000000000000 ) ) ;
#2003 = CIRCLE ( 'NONE', #240, 22.99899999999999523 ) ;
#2004 = DIRECTION ( 'NONE',  ( 1.000000000000000000, 0.000000000000000000, 0.000000000000000000 ) ) ;
#2005 = VERTEX_POINT ( 'NONE', #11088 ) ;
#2006 = DIRECTION ( 'NONE',  ( 0.000000000000000000, 0.000000000000000000, 1.000000000000000000 ) ) ;
#2007 = CARTESIAN_POINT ( 'NONE',  ( 3.000000000000000888, -22.42251312757882786, 5.117118920208413968 ) ) ;
#2008 = DIRECTION ( 'NONE',  ( 0.000000000000000000, 0.000000000000000000, 1.000000000000000000 ) ) ;
#2009 = CARTESIAN_POINT ( 'NONE',  ( -13.29946171776798280, 6.562258890817371793, 3.747395293195558847E-16 ) ) ;
#2010 = VECTOR ( 'NONE', #9725, 1000.000000000000000 ) ;
#2011 = DIRECTION ( 'NONE',  ( -1.000000000000000000, 0.000000000000000000, 0.000000000000000000 ) ) ;
#2012 = EDGE_CURVE ( 'NONE', #5418, #3455, #8821, .T. ) ;
#2013 = ORIENTED_EDGE ( 'NONE', *, *, #8582, .T. ) ;
#2014 = ORIENTED_EDGE ( 'NONE', *, *, #6579, .T. ) ;
#2015 = AXIS2_PLACEMENT_3D ( 'NONE', #5362, #10868, #576 ) ;
#2016 = DIRECTION ( 'NONE',  ( 0.000000000000000000, 0.000000000000000000, 1.000000000000000000 ) ) ;
#2017 = ORIENTED_EDGE ( 'NONE', *, *, #3256, .T. ) ;
#2018 = DIRECTION ( 'NONE',  ( -1.000000000000000000, -0.000000000000000000, 0.000000000000000000 ) ) ;
#2019 = AXIS2_PLACEMENT_3D ( 'NONE', #541, #783, #6240 ) ;
#2020 = DIRECTION ( 'NONE',  ( -1.000000000000000000, 0.000000000000000000, -0.000000000000000000 ) ) ;
#2021 = VERTEX_POINT ( 'NONE', #11151 ) ;
#2022 = EDGE_CURVE ( 'NONE', #8329, #2802, #2767, .T. ) ;
#2023 = LINE ( 'NONE', #1051, #9639 ) ;
#2024 = CIRCLE ( 'NONE', #7286, 9.599999999999997868 ) ;
#2025 = EDGE_CURVE ( 'NONE', #6334, #10386, #3812, .T. ) ;
#2026 = CARTESIAN_POINT ( 'NONE',  ( 3.000000000000000888, 20.86861857134747922, -9.667200211209612704 ) ) ;
#2027 = CARTESIAN_POINT ( 'NONE',  ( -15.85416723795448846, 2.087521067385502693, 6.857782953271941950E-17 ) ) ;
#2028 = CYLINDRICAL_SURFACE ( 'NONE', #8632, 9.599999999999997868 ) ;
#2029 = CYLINDRICAL_SURFACE ( 'NONE', #1026, 24.80000000000000071 ) ;
#2030 = AXIS2_PLACEMENT_3D ( 'NONE', #2475, #10803, #5807 ) ;
#2031 = ORIENTED_EDGE ( 'NONE', *, *, #7774, .F. ) ;
#2032 = ORIENTED_EDGE ( 'NONE', *, *, #8017, .T. ) ;
#2033 = LINE ( 'NONE', #3196, #3330 ) ;
#2034 = ORIENTED_EDGE ( 'NONE', *, *, #11659, .T. ) ;
#2035 = CARTESIAN_POINT ( 'NONE',  ( 2.839002905302877799, -15.63284973865751049, 10.00000000000000000 ) ) ;
#2036 = ADVANCED_FACE ( 'NONE', ( #2833 ), #6326, .T. ) ;
#2037 = DIRECTION ( 'NONE',  ( -1.000000000000000000, 0.000000000000000000, 0.000000000000000000 ) ) ;
#2038 = FILL_AREA_STYLE_COLOUR ( '', #9398 ) ;
#2039 = CARTESIAN_POINT ( 'NONE',  ( 16.47843063274904196, -5.593696103119284224, 6.857782953271941950E-17 ) ) ;
#2040 = ORIENTED_EDGE ( 'NONE', *, *, #11742, .T. ) ;
#2041 = AXIS2_PLACEMENT_3D ( 'NONE', #1068, #2043, #5654 ) ;
#2042 = DIRECTION ( 'NONE',  ( -1.000000000000000000, -0.000000000000000000, 0.000000000000000000 ) ) ;
#2043 = DIRECTION ( 'NONE',  ( 1.000000000000000000, 0.000000000000000000, 0.000000000000000000 ) ) ;
#2044 = CARTESIAN_POINT ( 'NONE',  ( 5.564773995946421969, -12.83798980516408683, 10.00000000000000000 ) ) ;
#2045 = CARTESIAN_POINT ( 'NONE',  ( 0.000000000000000000, -21.14796121233190362, -9.039786367039052806 ) ) ;
#2046 = CARTESIAN_POINT ( 'NONE',  ( 1.500000000000000444, -24.77821629063820907, -1.039229259764747004 ) ) ;
#2047 = CARTESIAN_POINT ( 'NONE',  ( 3.000000000000000888, 6.779701584702736206, 21.97702544527760082 ) ) ;
#2048 = EDGE_CURVE ( 'NONE', #7011, #246, #10570, .T. ) ;
#2049 = DIRECTION ( 'NONE',  ( 1.000000000000000000, -0.000000000000000000, 0.000000000000000000 ) ) ;
#2050 = AXIS2_PLACEMENT_3D ( 'NONE', #10605, #10721, #2398 ) ;
#2051 = ORIENTED_EDGE ( 'NONE', *, *, #7677, .T. ) ;
#2052 = EDGE_CURVE ( 'NONE', #2472, #5179, #7, .T. ) ;
#2053 = CARTESIAN_POINT ( 'NONE',  ( 0.000000000000000000, 15.13242714128119459, 17.31945870441152380 ) ) ;
#2054 = CARTESIAN_POINT ( 'NONE',  ( 6.563569809674243416, -3.208372544468512721, 10.00000000000000000 ) ) ;
#2055 = CARTESIAN_POINT ( 'NONE',  ( 3.000000000000000888, 20.41249101028211754, -9.589108953447965433 ) ) ;
#2056 = CARTESIAN_POINT ( 'NONE',  ( -7.130211940009574256, -7.605417807865423541, 10.00000000000000000 ) ) ;
#2057 = CARTESIAN_POINT ( 'NONE',  ( 7.525577113297162946, 13.03378399180780534, 6.857782953271941950E-17 ) ) ;
#2058 = EDGE_CURVE ( 'NONE', #8966, #3995, #7638, .T. ) ;
#2059 = DIRECTION ( 'NONE',  ( 0.000000000000000000, 0.4999999999999950040, 0.8660254037844415942 ) ) ;
#2060 = EDGE_LOOP ( 'NONE', ( #4600, #1218, #10442, #2040 ) ) ;
#2061 = VERTEX_POINT ( 'NONE', #5643 ) ;
#2062 = CARTESIAN_POINT ( 'NONE',  ( 0.000000000000000000, 0.000000000000000000, -15.00000000000000000 ) ) ;
#2063 = CIRCLE ( 'NONE', #3232, 24.80000000000000071 ) ;
#2064 = LINE ( 'NONE', #10323, #4912 ) ;
#2065 = ORIENTED_EDGE ( 'NONE', *, *, #4728, .T. ) ;
#2066 = DIRECTION ( 'NONE',  ( -1.000000000000000000, 0.000000000000000000, 0.000000000000000000 ) ) ;
#2067 = CARTESIAN_POINT ( 'NONE',  ( 0.03696586647634135525, -4.250492970015754324, 2.216586794261376644E-16 ) ) ;
#2068 = ADVANCED_FACE ( 'NONE', ( #9373 ), #808, .T. ) ;
#2069 = DIRECTION ( 'NONE',  ( 0.000000000000000000, 0.4067366430757948792, 0.9135454576426033091 ) ) ;
#2070 = CARTESIAN_POINT ( 'NONE',  ( -5.008276813248563997, -11.55791719732261313, 3.747395293195558847E-16 ) ) ;
#2071 = VECTOR ( 'NONE', #5339, 1000.000000000000000 ) ;
#2072 = CARTESIAN_POINT ( 'NONE',  ( -4.500000000000000000, 0.4999999999999998890, 3.000000000000000000 ) ) ;
#2073 = VERTEX_POINT ( 'NONE', #7531 ) ;
#2074 = ORIENTED_EDGE ( 'NONE', *, *, #7931, .T. ) ;
#2075 = SHAPE_DEFINITION_REPRESENTATION ( #5024, #7555 ) ;
#2076 = CARTESIAN_POINT ( 'NONE',  ( 0.2749788638910979355, -16.81181333738675931, 10.00000000000000000 ) ) ;
#2077 = ORIENTED_EDGE ( 'NONE', *, *, #1425, .F. ) ;
#2078 = CARTESIAN_POINT ( 'NONE',  ( 3.000000000000000888, -6.168200451485917668, 24.02068490260610645 ) ) ;
#2079 = LINE ( 'NONE', #5816, #7884 ) ;
#2080 = CARTESIAN_POINT ( 'NONE',  ( 3.000000000000000888, 0.000000000000000000, 0.000000000000000000 ) ) ;
#2081 = AXIS2_PLACEMENT_3D ( 'NONE', #4601, #11754, #9123 ) ;
#2082 = VERTEX_POINT ( 'NONE', #2592 ) ;
#2083 = DIRECTION ( 'NONE',  ( 0.000000000000000000, 0.000000000000000000, 1.000000000000000000 ) ) ;
#2084 = DIRECTION ( 'NONE',  ( 0.000000000000000000, 0.9945218953682729568, 0.1045284632676570929 ) ) ;
#2085 = CARTESIAN_POINT ( 'NONE',  ( -12.59589084681760518, 2.937805917057593863, 6.857782953271941950E-17 ) ) ;
#2086 = DIRECTION ( 'NONE',  ( 1.000000000000000000, 0.000000000000000000, 0.000000000000000000 ) ) ;
#2087 = ORIENTED_EDGE ( 'NONE', *, *, #9712, .T. ) ;
#2088 = CARTESIAN_POINT ( 'NONE',  ( 3.000000000000000888, 19.75591328264900781, -10.87771529938142123 ) ) ;
#2089 = ORIENTED_EDGE ( 'NONE', *, *, #7426, .F. ) ;
#2090 = CARTESIAN_POINT ( 'NONE',  ( 1.499999999999999556, -20.93895013827591001, 13.28910708463121360 ) ) ;
#2091 = EDGE_CURVE ( 'NONE', #712, #429, #743, .T. ) ;
#2092 = ORIENTED_EDGE ( 'NONE', *, *, #6618, .T. ) ;
#2093 = ADVANCED_FACE ( 'NONE', ( #11034 ), #10103, .T. ) ;
#2094 = CARTESIAN_POINT ( 'NONE',  ( -1.036640877615905287, -15.73686152240404823, 10.00000000000000000 ) ) ;
#2095 = CARTESIAN_POINT ( 'NONE',  ( 3.000000000000000888, 21.30300407174352983, 7.402892494506653875 ) ) ;
#2096 =( NAMED_UNIT ( * ) SI_UNIT ( $, .STERADIAN. ) SOLID_ANGLE_UNIT ( ) );
#2097 = DIRECTION ( 'NONE',  ( -1.000000000000000000, 0.000000000000000000, 0.000000000000000000 ) ) ;
#2098 = DIRECTION ( 'NONE',  ( 0.000000000000000000, 0.4067366430757948792, 0.9135454576426033091 ) ) ;
#2099 = CARTESIAN_POINT ( 'NONE',  ( -11.39998097177319636, 5.856612080558658562, 10.00000000000000000 ) ) ;
#2100 = DIRECTION ( 'NONE',  ( 0.000000000000000000, -0.9510565162951504226, -0.3090169943749574433 ) ) ;
#2101 = CARTESIAN_POINT ( 'NONE',  ( 0.4634152073531430105, 14.27464310366533340, 3.747395293195558847E-16 ) ) ;
#2102 = ADVANCED_FACE ( 'NONE', ( #10529 ), #3991, .T. ) ;
#2103 = CYLINDRICAL_SURFACE ( 'NONE', #8012, 19.99999999999999645 ) ;
#2104 = VERTEX_POINT ( 'NONE', #9619 ) ;
#2105 = DIRECTION ( 'NONE',  ( 0.000000000000000000, -0.2079116908177665313, 0.9781476007338041345 ) ) ;
#2106 = ADVANCED_FACE ( 'NONE', ( #3927 ), #5026, .T. ) ;
#2107 = ORIENTED_EDGE ( 'NONE', *, *, #4414, .T. ) ;
#2108 = VECTOR ( 'NONE', #3820, 1000.000000000000000 ) ;
#2109 = DIRECTION ( 'NONE',  ( 0.000000000000000000, 0.000000000000000000, 1.000000000000000000 ) ) ;
#2110 = CARTESIAN_POINT ( 'NONE',  ( -5.319913005755715574, -3.351504787099933047, 10.00000000000000000 ) ) ;
#2111 = DIRECTION ( 'NONE',  ( 1.000000000000000000, 0.000000000000000000, 0.000000000000000000 ) ) ;
#2112 = CARTESIAN_POINT ( 'NONE',  ( 8.393308867179015920, -1.106660293010312657, 10.00000000000000000 ) ) ;
#2113 = CARTESIAN_POINT ( 'NONE',  ( 14.27634331491212016, 3.322769473268863738, 6.857782953271941950E-17 ) ) ;
#2114 = DIRECTION ( 'NONE',  ( -1.000000000000000000, 0.000000000000000000, 0.000000000000000000 ) ) ;
#2115 = EDGE_CURVE ( 'NONE', #2610, #9943, #1189, .T. ) ;
#2116 = ORIENTED_EDGE ( 'NONE', *, *, #10951, .F. ) ;
#2117 = ORIENTED_EDGE ( 'NONE', *, *, #2320, .T. ) ;
#2118 = CARTESIAN_POINT ( 'NONE',  ( 22.00000000000000000, 2.694222958124176809E-15, 0.000000000000000000 ) ) ;
#2119 = DIRECTION ( 'NONE',  ( 0.000000000000000000, -0.6691306063588644548, 0.7431448254773886930 ) ) ;
#2120 = AXIS2_PLACEMENT_3D ( 'NONE', #3280, #5240, #11722 ) ;
#2121 = FACE_OUTER_BOUND ( 'NONE', #9248, .T. ) ;
#2122 = CYLINDRICAL_SURFACE ( 'NONE', #6223, 24.80000000000000071 ) ;
#2123 = CIRCLE ( 'NONE', #11311, 9.599999999999996092 ) ;
#2124 = CARTESIAN_POINT ( 'NONE',  ( 10.51453309316909213, -0.3307463982597989571, 3.747395293195558847E-16 ) ) ;
#2125 = EDGE_CURVE ( 'NONE', #6397, #4202, #122, .T. ) ;
#2126 = LINE ( 'NONE', #10576, #12103 ) ;
#2127 = AXIS2_PLACEMENT_3D ( 'NONE', #12096, #12038, #11690 ) ;
#2128 = ORIENTED_EDGE ( 'NONE', *, *, #3793, .F. ) ;
#2129 = EDGE_LOOP ( 'NONE', ( #4383, #10291 ) ) ;
#2130 = DIRECTION ( 'NONE',  ( 1.000000000000000000, 0.000000000000000000, 0.000000000000000000 ) ) ;
#2131 = CARTESIAN_POINT ( 'NONE',  ( 11.73504485001147835, -12.52947377801879192, 10.00000000000000000 ) ) ;
#2132 = VERTEX_POINT ( 'NONE', #6613 ) ;
#2133 = DIRECTION ( 'NONE',  ( 0.000000000000000000, 0.000000000000000000, 1.000000000000000000 ) ) ;
#2134 = CARTESIAN_POINT ( 'NONE',  ( 0.000000000000000000, 0.000000000000000000, 20.00000000000000000 ) ) ;
#2135 = ADVANCED_FACE ( 'NONE', ( #7770, #180 ), #7655, .T. ) ;
#2136 = CARTESIAN_POINT ( 'NONE',  ( 1.500000000000000444, 11.48910920600714469, -21.97817939804027176 ) ) ;
#2137 = ORIENTED_EDGE ( 'NONE', *, *, #8799, .F. ) ;
#2138 = CIRCLE ( 'NONE', #5658, 24.80000000000000071 ) ;
#2139 = AXIS2_PLACEMENT_3D ( 'NONE', #7625, #2990, #6713 ) ;
#2140 = CARTESIAN_POINT ( 'NONE',  ( 0.000000000000000000, -23.88662356770110762, -6.668524164681871369 ) ) ;
#2141 = AXIS2_PLACEMENT_3D ( 'NONE', #5008, #11728, #7818 ) ;
#2142 = DIRECTION ( 'NONE',  ( 0.000000000000000000, 0.000000000000000000, 1.000000000000000000 ) ) ;
#2143 = CARTESIAN_POINT ( 'NONE',  ( -16.06046882360139350, -0.5196555361422402486, 6.857782953271941950E-17 ) ) ;
#2144 = CARTESIAN_POINT ( 'NONE',  ( 0.000000000000000000, -11.20082935824089354, 20.08719549084861455 ) ) ;
#2145 = ORIENTED_EDGE ( 'NONE', *, *, #10045, .T. ) ;
#2146 = DIRECTION ( 'NONE',  ( 1.000000000000000000, 0.000000000000000000, 0.000000000000000000 ) ) ;
#2147 = VERTEX_POINT ( 'NONE', #6674 ) ;
#2148 = ORIENTED_EDGE ( 'NONE', *, *, #10394, .F. ) ;
#2149 = DIRECTION ( 'NONE',  ( -1.000000000000000000, 0.000000000000000000, -0.000000000000000000 ) ) ;
#2150 = ORIENTED_EDGE ( 'NONE', *, *, #11846, .T. ) ;
#2151 = CARTESIAN_POINT ( 'NONE',  ( 5.172292865810427465, -11.91455349003027919, 10.00000000000000000 ) ) ;
#2152 = AXIS2_PLACEMENT_3D ( 'NONE', #4061, #3263, #1613 ) ;
#2153 = DIRECTION ( 'NONE',  ( 1.000000000000000000, 0.000000000000000000, 0.000000000000000000 ) ) ;
#2154 = SURFACE_STYLE_FILL_AREA ( #10536 ) ;
#2155 = APPLICATION_CONTEXT ( 'automotive_design' ) ;
#2156 = DIRECTION ( 'NONE',  ( -1.000000000000000000, -0.000000000000000000, 0.000000000000000000 ) ) ;
#2157 = FACE_OUTER_BOUND ( 'NONE', #1552, .T. ) ;
#2158 = CARTESIAN_POINT ( 'NONE',  ( -12.59589084681761229, 2.937805917057824789, 10.00000000000000000 ) ) ;
#2159 = CIRCLE ( 'NONE', #11542, 9.599999999999997868 ) ;
#2160 = FACE_OUTER_BOUND ( 'NONE', #70, .T. ) ;
#2161 = CARTESIAN_POINT ( 'NONE',  ( 1.499999999999999556, 24.53384959170462665, -3.623565124516855640 ) ) ;
#2162 = AXIS2_PLACEMENT_3D ( 'NONE', #8154, #7163, #4241 ) ;
#2163 = DIRECTION ( 'NONE',  ( 0.000000000000000000, 0.000000000000000000, 1.000000000000000000 ) ) ;
#2164 = CYLINDRICAL_SURFACE ( 'NONE', #8214, 22.99899999999999878 ) ;
#2165 = ORIENTED_EDGE ( 'NONE', *, *, #2658, .T. ) ;
#2166 = VECTOR ( 'NONE', #10232, 1000.000000000000000 ) ;
#2167 = CARTESIAN_POINT ( 'NONE',  ( 3.000000000000000888, 22.54798042742718067, 9.142421143074731305 ) ) ;
#2168 = CARTESIAN_POINT ( 'NONE',  ( -2.296015608618633852, -6.188270089872266233, 10.00000000000000000 ) ) ;
#2169 = VECTOR ( 'NONE', #11989, 1000.000000000000000 ) ;
#2170 = ADVANCED_FACE ( 'NONE', ( #8646 ), #3073, .F. ) ;
#2171 = DIRECTION ( 'NONE',  ( 0.000000000000000000, 0.000000000000000000, -1.000000000000000000 ) ) ;
#2172 = EDGE_CURVE ( 'NONE', #1367, #5220, #2562, .T. ) ;
#2173 = CARTESIAN_POINT ( 'NONE',  ( -0.1814876354083667931, -10.77628937513455654, 10.00000000000000000 ) ) ;
#2174 = CARTESIAN_POINT ( 'NONE',  ( 14.53830338343599848, -0.2437330612273620467, 6.857782953271941950E-17 ) ) ;
#2175 = EDGE_CURVE ( 'NONE', #9118, #11061, #11358, .T. ) ;
#2176 = DIRECTION ( 'NONE',  ( 0.000000000000000000, -0.9135454576426046414, 0.4067366430757920481 ) ) ;
#2177 = CIRCLE ( 'NONE', #6094, 9.599999999999997868 ) ;
#2178 = DIRECTION ( 'NONE',  ( -1.000000000000000000, 0.000000000000000000, -0.000000000000000000 ) ) ;
#2179 = ORIENTED_EDGE ( 'NONE', *, *, #5689, .T. ) ;
#2180 = VECTOR ( 'NONE', #8739, 1000.000000000000000 ) ;
#2181 = EDGE_LOOP ( 'NONE', ( #5177, #2087, #5827, #4027 ) ) ;
#2182 = FACE_OUTER_BOUND ( 'NONE', #5458, .T. ) ;
#2183 = CARTESIAN_POINT ( 'NONE',  ( 15.52845182490561626, -5.270724383582042982, 10.00000000000000000 ) ) ;
#2184 = VECTOR ( 'NONE', #3030, 1000.000000000000000 ) ;
#2185 = PRODUCT ( 'arbor', 'arbor', '', ( #4393 ) ) ;
#2186 = FACE_OUTER_BOUND ( 'NONE', #645, .T. ) ;
#2187 = CARTESIAN_POINT ( 'NONE',  ( 20.00000000000000000, 0.000000000000000000, -5.000000000000000000 ) ) ;
#2188 = AXIS2_PLACEMENT_3D ( 'NONE', #10952, #10274, #1892 ) ;
#2189 = CARTESIAN_POINT ( 'NONE',  ( -11.15100792855598755, -5.055838994807843711, 3.747395293195558847E-16 ) ) ;
#2190 = AXIS2_PLACEMENT_3D ( 'NONE', #6040, #9372, #7717 ) ;
#2191 = DIRECTION ( 'NONE',  ( 0.000000000000000000, 0.000000000000000000, -1.000000000000000000 ) ) ;
#2192 = ORIENTED_EDGE ( 'NONE', *, *, #9874, .F. ) ;
#2193 = CIRCLE ( 'NONE', #8251, 22.99899999999999878 ) ;
#2194 = ORIENTED_EDGE ( 'NONE', *, *, #8938, .T. ) ;
#2195 = APPLICATION_PROTOCOL_DEFINITION ( 'draft international standard', 'automotive_design', 1998, #10355 ) ;
#2196 = CARTESIAN_POINT ( 'NONE',  ( 1.748316258820582947, 15.14524454193559144, 10.00000000000000000 ) ) ;
#2197 = ORIENTED_EDGE ( 'NONE', *, *, #7960, .F. ) ;
#2198 = CARTESIAN_POINT ( 'NONE',  ( 3.000000000000000888, 2.062268319295869290, -22.90635393027944033 ) ) ;
#2199 = FACE_OUTER_BOUND ( 'NONE', #949, .T. ) ;
#2200 = ADVANCED_FACE ( 'NONE', ( #6789 ), #5885, .T. ) ;
#2201 = CYLINDRICAL_SURFACE ( 'NONE', #10292, 9.599999999999997868 ) ;
#2202 = ORIENTED_EDGE ( 'NONE', *, *, #6230, .T. ) ;
#2203 = CARTESIAN_POINT ( 'NONE',  ( 3.000000000000000888, 22.47229024614980020, -1.901833551798019162 ) ) ;
#2204 = DIRECTION ( 'NONE',  ( -1.000000000000000000, -0.000000000000000000, -0.000000000000000000 ) ) ;
#2205 = CARTESIAN_POINT ( 'NONE',  ( -12.91830213043053988, -2.344901317288421883, 6.857782953271941950E-17 ) ) ;
#2206 = AXIS2_PLACEMENT_3D ( 'NONE', #1984, #11345, #133 ) ;
#2207 = ORIENTED_EDGE ( 'NONE', *, *, #9421, .F. ) ;
#2208 = ADVANCED_FACE ( 'NONE', ( #307 ), #9492, .T. ) ;
#2209 = LINE ( 'NONE', #5710, #1 ) ;
#2210 = EDGE_LOOP ( 'NONE', ( #4328, #11960, #9693, #7652 ) ) ;
#2211 = CYLINDRICAL_SURFACE ( 'NONE', #6653, 24.80000000000000071 ) ;
#2212 = VERTEX_POINT ( 'NONE', #364 ) ;
#2213 = VECTOR ( 'NONE', #7893, 1000.000000000000000 ) ;
#2214 = CARTESIAN_POINT ( 'NONE',  ( 7.078846155420733588, 8.354583459611244933, 10.00000000000000000 ) ) ;
#2215 = VECTOR ( 'NONE', #5616, 1000.000000000000000 ) ;
#2216 = AXIS2_PLACEMENT_3D ( 'NONE', #2134, #10519, #10760 ) ;
#2217 = FACE_OUTER_BOUND ( 'NONE', #8088, .T. ) ;
#2218 = SHAPE_REPRESENTATION_RELATIONSHIP ( 'NONE' , 'NONE' ,  #8353, #2941 ) ;
#2219 = DIRECTION ( 'NONE',  ( 0.000000000000000000, 0.000000000000000000, 1.000000000000000000 ) ) ;
#2220 = EDGE_CURVE ( 'NONE', #10972, #4464, #2209, .T. ) ;
#2221 = DIRECTION ( 'NONE',  ( -1.000000000000000000, 0.000000000000000000, 0.000000000000000000 ) ) ;
#2222 = CARTESIAN_POINT ( 'NONE',  ( 11.20109743375192224, 9.815261043520028039, 10.00000000000000000 ) ) ;
#2223 = CIRCLE ( 'NONE', #8865, 22.99900000000000233 ) ;
#2224 = DIRECTION ( 'NONE',  ( -1.000000000000000000, 0.000000000000000000, -0.000000000000000000 ) ) ;
#2225 = FACE_OUTER_BOUND ( 'NONE', #1631, .T. ) ;
#2226 = DIRECTION ( 'NONE',  ( 0.000000000000000000, 0.000000000000000000, 1.000000000000000000 ) ) ;
#2227 = DIRECTION ( 'NONE',  ( -1.000000000000000000, 0.000000000000000000, 0.000000000000000000 ) ) ;
#2228 = ORIENTED_EDGE ( 'NONE', *, *, #3598, .F. ) ;
#2229 = VERTEX_POINT ( 'NONE', #5948 ) ;
#2230 = ORIENTED_EDGE ( 'NONE', *, *, #9945, .T. ) ;
#2231 = AXIS2_PLACEMENT_3D ( 'NONE', #11166, #11341, #11286 ) ;
#2232 = DIRECTION ( 'NONE',  ( 0.000000000000000000, 0.000000000000000000, 1.000000000000000000 ) ) ;
#2233 = CYLINDRICAL_SURFACE ( 'NONE', #3504, 22.99899999999999878 ) ;
#2234 = CARTESIAN_POINT ( 'NONE',  ( 6.986659217179110648, 9.748146710219847577, 10.00000000000000000 ) ) ;
#2235 = CARTESIAN_POINT ( 'NONE',  ( 8.588976300537435549, -11.19439025337200810, 6.857782953271941950E-17 ) ) ;
#2236 = CIRCLE ( 'NONE', #2632, 22.99899999999999878 ) ;
#2237 = CARTESIAN_POINT ( 'NONE',  ( 3.000000000000000888, -18.51065745848386968, 12.88318129270172818 ) ) ;
#2238 = ORIENTED_EDGE ( 'NONE', *, *, #2480, .T. ) ;
#2239 = ORIENTED_EDGE ( 'NONE', *, *, #1092, .T. ) ;
#2240 = EDGE_CURVE ( 'NONE', #6844, #8735, #8583, .T. ) ;
#2241 = ORIENTED_EDGE ( 'NONE', *, *, #4648, .T. ) ;
#2242 = DIRECTION ( 'NONE',  ( 0.000000000000000000, 0.000000000000000000, -1.000000000000000000 ) ) ;
#2243 = ADVANCED_FACE ( 'NONE', ( #5769 ), #4785, .T. ) ;
#2244 = DIRECTION ( 'NONE',  ( 0.000000000000000000, 0.000000000000000000, 1.000000000000000000 ) ) ;
#2245 = ADVANCED_FACE ( 'NONE', ( #10411 ), #2029, .T. ) ;
#2246 = ORIENTED_EDGE ( 'NONE', *, *, #10256, .T. ) ;
#2247 = DIRECTION ( 'NONE',  ( 0.000000000000000000, 0.8090169943749486725, -0.5877852522924714718 ) ) ;
#2248 = DIRECTION ( 'NONE',  ( -1.000000000000000000, -0.000000000000000000, -0.000000000000000000 ) ) ;
#2249 = CARTESIAN_POINT ( 'NONE',  ( -5.868204859621548586, -7.421994279450896848, 3.747395293195558847E-16 ) ) ;
#2250 = EDGE_CURVE ( 'NONE', #6885, #5042, #544, .T. ) ;
#2251 = DIRECTION ( 'NONE',  ( 1.000000000000000000, 0.000000000000000000, 0.000000000000000000 ) ) ;
#2252 = VERTEX_POINT ( 'NONE', #6913 ) ;
#2253 = VERTEX_POINT ( 'NONE', #7952 ) ;
#2254 = AXIS2_PLACEMENT_3D ( 'NONE', #11771, #1258, #6024 ) ;
#2255 = DIRECTION ( 'NONE',  ( 0.000000000000000000, 1.000000000000000000, 0.000000000000000000 ) ) ;
#2256 = CARTESIAN_POINT ( 'NONE',  ( 13.14573027368779456, 6.745762002080610387, 10.00000000000000000 ) ) ;
#2257 = ORIENTED_EDGE ( 'NONE', *, *, #11298, .T. ) ;
#2258 = CARTESIAN_POINT ( 'NONE',  ( 3.000000000000000888, -8.753070780933015271, -20.78471918669869467 ) ) ;
#2259 = CARTESIAN_POINT ( 'NONE',  ( 17.50000000000000000, 0.000000000000000000, 10.00000000000000000 ) ) ;
#2260 = FACE_OUTER_BOUND ( 'NONE', #2060, .T. ) ;
#2261 = ORIENTED_EDGE ( 'NONE', *, *, #1425, .T. ) ;
#2262 = FACE_OUTER_BOUND ( 'NONE', #3512, .T. ) ;
#2263 = EDGE_CURVE ( 'NONE', #10872, #1804, #11184, .T. ) ;
#2264 = AXIS2_PLACEMENT_3D ( 'NONE', #937, #4231, #2334 ) ;
#2265 = DIRECTION ( 'NONE',  ( 0.000000000000000000, 0.000000000000000000, 1.000000000000000000 ) ) ;
#2266 = CARTESIAN_POINT ( 'NONE',  ( 11.40744677810890373, -1.317628706759688129, 6.857782953271941950E-17 ) ) ;
#2267 = EDGE_LOOP ( 'NONE', ( #4964, #1999, #2034, #3151 ) ) ;
#2268 = EDGE_CURVE ( 'NONE', #6248, #9359, #1214, .T. ) ;
#2269 = CARTESIAN_POINT ( 'NONE',  ( 50.00005079999999680, 4.898587196589412829E-16, -4.000000000000000000 ) ) ;
#2270 = LINE ( 'NONE', #5829, #5879 ) ;
#2271 = ORIENTED_EDGE ( 'NONE', *, *, #5420, .F. ) ;
#2272 = AXIS2_PLACEMENT_3D ( 'NONE', #10040, #868, #1661 ) ;
#2273 = CARTESIAN_POINT ( 'NONE',  ( -0.1481022647113163504, -9.773457036294484368, 10.00000000000000000 ) ) ;
#2274 = DIRECTION ( 'NONE',  ( 1.000000000000000000, 1.445602896647339163E-16, 0.000000000000000000 ) ) ;
#2275 = EDGE_CURVE ( 'NONE', #8500, #3964, #8456, .T. ) ;
#2276 = CARTESIAN_POINT ( 'NONE',  ( 3.000000000000000888, -11.20082935824061110, -20.08719549084876732 ) ) ;
#2277 = CARTESIAN_POINT ( 'NONE',  ( 0.000000000000000000, -4.135161237383746524, 24.45282072769599679 ) ) ;
#2278 = CARTESIAN_POINT ( 'NONE',  ( -10.84705874452746777, 6.751620637726422736, 10.00000000000000000 ) ) ;
#2279 = VECTOR ( 'NONE', #5383, 1000.000000000000000 ) ;
#2280 = CYLINDRICAL_SURFACE ( 'NONE', #11572, 24.80000000000000071 ) ;
#2281 = CARTESIAN_POINT ( 'NONE',  ( 0.000000000000000000, -14.74749645580022772, 17.06259499759939402 ) ) ;
#2282 = EDGE_CURVE ( 'NONE', #1912, #6126, #4346, .T. ) ;
#2283 = CYLINDRICAL_SURFACE ( 'NONE', #7028, 1.500000000000000222 ) ;
#2284 = VERTEX_POINT ( 'NONE', #11576 ) ;
#2285 = DIRECTION ( 'NONE',  ( 0.000000000000000000, -0.4999999999999887867, -0.8660254037844452579 ) ) ;
#2286 = ORIENTED_EDGE ( 'NONE', *, *, #1989, .F. ) ;
#2287 = DIRECTION ( 'NONE',  ( -1.000000000000000000, -0.000000000000000000, 0.000000000000000000 ) ) ;
#2288 = EDGE_CURVE ( 'NONE', #4846, #11898, #486, .T. ) ;
#2289 = DIRECTION ( 'NONE',  ( -1.000000000000000000, -0.000000000000000000, -0.000000000000000000 ) ) ;
#2290 = DIRECTION ( 'NONE',  ( -1.000000000000000000, 0.000000000000000000, 0.000000000000000000 ) ) ;
#2291 = CARTESIAN_POINT ( 'NONE',  ( 11.50231346626665996, 1.508968394323198847, 10.00000000000000000 ) ) ;
#2292 = CARTESIAN_POINT ( 'NONE',  ( 1.597090680284417363, 12.12373805211590749, 6.857782953271941950E-17 ) ) ;
#2293 = LINE ( 'NONE', #3163, #10586 ) ;
#2294 = CARTESIAN_POINT ( 'NONE',  ( 0.000000000000000000, 0.000000000000000000, 3.000000000000000000 ) ) ;
#2295 = AXIS2_PLACEMENT_3D ( 'NONE', #11427, #1549, #216 ) ;
#2296 = ORIENTED_EDGE ( 'NONE', *, *, #6795, .F. ) ;
#2297 = AXIS2_PLACEMENT_3D ( 'NONE', #570, #452, #6089 ) ;
#2298 = ORIENTED_EDGE ( 'NONE', *, *, #3148, .T. ) ;
#2299 = CARTESIAN_POINT ( 'NONE',  ( 0.000000000000000000, 20.78471918669872665, -8.753070780932940664 ) ) ;
#2300 = DIRECTION ( 'NONE',  ( -1.000000000000000000, -0.000000000000000000, -0.000000000000000000 ) ) ;
#2301 = CYLINDRICAL_SURFACE ( 'NONE', #1924, 9.599999999999997868 ) ;
#2302 = VECTOR ( 'NONE', #11462, 1000.000000000000000 ) ;
#2303 = CARTESIAN_POINT ( 'NONE',  ( -12.04643853703213452, -0.2059847383342608973, 3.747395293195558847E-16 ) ) ;
#2304 = EDGE_CURVE ( 'NONE', #11132, #1084, #2325, .T. ) ;
#2305 = EDGE_CURVE ( 'NONE', #1364, #4173, #3245, .T. ) ;
#2306 = CARTESIAN_POINT ( 'NONE',  ( 3.000000000000002665, 0.000000000000000000, 0.000000000000000000 ) ) ;
#2307 = ORIENTED_EDGE ( 'NONE', *, *, #4636, .F. ) ;
#2308 = VERTEX_POINT ( 'NONE', #8822 ) ;
#2309 = CARTESIAN_POINT ( 'NONE',  ( 1.597090680284417807, 12.12373805211591460, 10.00000000000000000 ) ) ;
#2310 = VERTEX_POINT ( 'NONE', #4171 ) ;
#2311 = VECTOR ( 'NONE', #5927, 1000.000000000000000 ) ;
#2312 = EDGE_CURVE ( 'NONE', #10264, #11249, #10004, .T. ) ;
#2313 = VECTOR ( 'NONE', #6165, 1000.000000000000000 ) ;
#2314 = LINE ( 'NONE', #5069, #3108 ) ;
#2315 = CARTESIAN_POINT ( 'NONE',  ( -3.500000000000000000, 4.286263797015736595E-16, -15.00000000000000000 ) ) ;
#2316 = DIRECTION ( 'NONE',  ( 1.000000000000000000, 0.000000000000000000, -0.000000000000000000 ) ) ;
#2317 = VERTEX_POINT ( 'NONE', #7837 ) ;
#2318 = EDGE_CURVE ( 'NONE', #6367, #9845, #8645, .T. ) ;
#2319 = CARTESIAN_POINT ( 'NONE',  ( 3.000000000000000888, -13.28910708463113366, -20.93895013827595264 ) ) ;
#2320 = EDGE_CURVE ( 'NONE', #10471, #2327, #9034, .T. ) ;
#2321 = CARTESIAN_POINT ( 'NONE',  ( 3.000000000000000888, 0.000000000000000000, 0.000000000000000000 ) ) ;
#2322 = CARTESIAN_POINT ( 'NONE',  ( 7.334967666341834835, -8.371827447635054043, 6.857782953271941950E-17 ) ) ;
#2323 = AXIS2_PLACEMENT_3D ( 'NONE', #2487, #5183, #7245 ) ;
#2324 = EDGE_CURVE ( 'NONE', #8063, #7835, #8049, .T. ) ;
#2325 = LINE ( 'NONE', #2269, #223 ) ;
#2326 = ORIENTED_EDGE ( 'NONE', *, *, #7091, .T. ) ;
#2327 = VERTEX_POINT ( 'NONE', #2446 ) ;
#2328 = CARTESIAN_POINT ( 'NONE',  ( -10.00000000000000000, 0.000000000000000000, 0.000000000000000000 ) ) ;
#2329 = VERTEX_POINT ( 'NONE', #2388 ) ;
#2330 = CARTESIAN_POINT ( 'NONE',  ( 2.257301671556971367, -9.631158585656901749, 10.00000000000000000 ) ) ;
#2331 = AXIS2_PLACEMENT_3D ( 'NONE', #6956, #3236, #9667 ) ;
#2332 = VECTOR ( 'NONE', #7364, 1000.000000000000000 ) ;
#2333 = EDGE_LOOP ( 'NONE', ( #4156, #5133, #1265, #1708 ) ) ;
#2334 = DIRECTION ( 'NONE',  ( -1.000000000000000000, 0.000000000000000000, -0.000000000000000000 ) ) ;
#2335 = AXIS2_PLACEMENT_3D ( 'NONE', #2306, #10693, #5128 ) ;
#2336 = CARTESIAN_POINT ( 'NONE',  ( 0.000000000000000000, 0.000000000000000000, 1.000000000000000000 ) ) ;
#2337 = DIRECTION ( 'NONE',  ( 0.000000000000000000, -0.8090169943749406789, -0.5877852522924823520 ) ) ;
#2338 = CARTESIAN_POINT ( 'NONE',  ( 4.138106518799270717, 8.052838533163344081, 10.00000000000000000 ) ) ;
#2339 = DIRECTION ( 'NONE',  ( -1.000000000000000000, -0.000000000000000000, 0.000000000000000000 ) ) ;
#2340 = CARTESIAN_POINT ( 'NONE',  ( 13.53515989517831564, -0.2218654272304620700, 3.747395293195558847E-16 ) ) ;
#2341 = DIRECTION ( 'NONE',  ( 0.000000000000000000, 0.000000000000000000, 1.000000000000000000 ) ) ;
#2342 = DIRECTION ( 'NONE',  ( -1.000000000000000000, 0.000000000000000000, 0.000000000000000000 ) ) ;
#2343 = CIRCLE ( 'NONE', #3324, 9.599999999999997868 ) ;
#2344 = ORIENTED_EDGE ( 'NONE', *, *, #9652, .F. ) ;
#2345 = CARTESIAN_POINT ( 'NONE',  ( 17.49999999999999645, 0.000000000000000000, 6.857782953271941950E-17 ) ) ;
#2346 = VERTEX_POINT ( 'NONE', #6966 ) ;
#2347 = EDGE_CURVE ( 'NONE', #9529, #6518, #4151, .T. ) ;
#2348 = PLANE ( 'NONE',  #2297 ) ;
#2349 = CARTESIAN_POINT ( 'NONE',  ( 0.000000000000000000, 0.000000000000000000, 1.000000000000000000 ) ) ;
#2350 = CARTESIAN_POINT ( 'NONE',  ( -5.152979166089619589, -5.321787192520355703, 10.00000000000000000 ) ) ;
#2351 = CARTESIAN_POINT ( 'NONE',  ( -4.389456771235329846, 11.66511648340389051, 6.857782953271941950E-17 ) ) ;
#2352 = DIRECTION ( 'NONE',  ( 0.000000000000000000, 0.000000000000000000, 1.000000000000000000 ) ) ;
#2353 = DIRECTION ( 'NONE',  ( -1.000000000000000000, 0.000000000000000000, 0.000000000000000000 ) ) ;
#2354 = ORIENTED_EDGE ( 'NONE', *, *, #7955, .T. ) ;
#2355 = EDGE_CURVE ( 'NONE', #8745, #2754, #7862, .T. ) ;
#2356 = AXIS2_PLACEMENT_3D ( 'NONE', #11643, #6259, #5097 ) ;
#2357 = AXIS2_PLACEMENT_3D ( 'NONE', #289, #9478, #3798 ) ;
#2358 = AXIS2_PLACEMENT_3D ( 'NONE', #7457, #2820, #5389 ) ;
#2359 = ORIENTED_EDGE ( 'NONE', *, *, #10785, .F. ) ;
#2360 = AXIS2_PLACEMENT_3D ( 'NONE', #4830, #10513, #9481 ) ;
#2361 = DIRECTION ( 'NONE',  ( -1.000000000000000000, -0.000000000000000000, -0.000000000000000000 ) ) ;
#2362 = LINE ( 'NONE', #6103, #10517 ) ;
#2363 = CARTESIAN_POINT ( 'NONE',  ( 8.000000000000000000, 0.000000000000000000, 0.000000000000000000 ) ) ;
#2364 = CIRCLE ( 'NONE', #10177, 24.80000000000000071 ) ;
#2365 = AXIS2_PLACEMENT_3D ( 'NONE', #990, #4732, #8468 ) ;
#2366 = CIRCLE ( 'NONE', #4918, 9.599999999999997868 ) ;
#2367 = CARTESIAN_POINT ( 'NONE',  ( 2.467392210070199710, 7.745125807189173095, 3.747395293195558847E-16 ) ) ;
#2368 = CIRCLE ( 'NONE', #11752, 22.99899999999999878 ) ;
#2369 = CARTESIAN_POINT ( 'NONE',  ( 0.000000000000000000, 0.000000000000000000, 0.000000000000000000 ) ) ;
#2370 = DIRECTION ( 'NONE',  ( -1.000000000000000000, -0.000000000000000000, 0.000000000000000000 ) ) ;
#2371 = ORIENTED_EDGE ( 'NONE', *, *, #2312, .T. ) ;
#2372 = ORIENTED_EDGE ( 'NONE', *, *, #10243, .F. ) ;
#2373 = CARTESIAN_POINT ( 'NONE',  ( 2.578468386369561216, 11.91291369680097567, 10.00000000000000000 ) ) ;
#2374 = VECTOR ( 'NONE', #4855, 1000.000000000000000 ) ;
#2375 = ORIENTED_EDGE ( 'NONE', *, *, #3248, .T. ) ;
#2376 = CARTESIAN_POINT ( 'NONE',  ( 3.000000000000000888, -15.42759117534397006, 16.45023496161660148 ) ) ;
#2377 = DIRECTION ( 'NONE',  ( -1.000000000000000000, 0.000000000000000000, 0.000000000000000000 ) ) ;
#2378 = AXIS2_PLACEMENT_3D ( 'NONE', #4592, #7205, #2817 ) ;
#2379 = CARTESIAN_POINT ( 'NONE',  ( 1.500000000000000444, -24.53384959170454849, -3.623565124517358793 ) ) ;
#2380 = ORIENTED_EDGE ( 'NONE', *, *, #2571, .T. ) ;
#2381 = FACE_OUTER_BOUND ( 'NONE', #5079, .T. ) ;
#2382 = LINE ( 'NONE', #3241, #1803 ) ;
#2383 = CARTESIAN_POINT ( 'NONE',  ( 10.63538685525200478, -4.008487272325076844, 6.857782953271941950E-17 ) ) ;
#2384 = CIRCLE ( 'NONE', #2979, 22.99899999999999878 ) ;
#2385 = EDGE_CURVE ( 'NONE', #5574, #10348, #3141, .T. ) ;
#2386 = AXIS2_PLACEMENT_3D ( 'NONE', #2761, #8577, #7583 ) ;
#2387 = EDGE_LOOP ( 'NONE', ( #3785, #6172, #12021, #6330 ) ) ;
#2388 = CARTESIAN_POINT ( 'NONE',  ( 3.000000000000000888, -15.40502424595158537, 19.43515443678397503 ) ) ;
#2389 = LINE ( 'NONE', #10895, #9795 ) ;
#2390 = VERTEX_POINT ( 'NONE', #1411 ) ;
#2391 = CARTESIAN_POINT ( 'NONE',  ( -10.51222845931418703, 5.388985543801221745, 10.00000000000000000 ) ) ;
#2392 = ADVANCED_FACE ( 'NONE', ( #10894 ), #5204, .T. ) ;
#2393 = VERTEX_POINT ( 'NONE', #3436 ) ;
#2394 = CYLINDRICAL_SURFACE ( 'NONE', #3836, 22.99899999999999878 ) ;
#2395 = CARTESIAN_POINT ( 'NONE',  ( 3.000000000000000888, 22.21333432029578248, -11.02759168516722887 ) ) ;
#2396 = EDGE_CURVE ( 'NONE', #10386, #10594, #993, .T. ) ;
#2397 = DIRECTION ( 'NONE',  ( -1.000000000000000000, 0.000000000000000000, -0.000000000000000000 ) ) ;
#2398 = DIRECTION ( 'NONE',  ( 1.000000000000000000, 0.000000000000000000, 0.000000000000000000 ) ) ;
#2399 = CARTESIAN_POINT ( 'NONE',  ( -2.764021070441486039, -10.29567250283336399, 10.00000000000000000 ) ) ;
#2400 = DIRECTION ( 'NONE',  ( 0.000000000000000000, 0.000000000000000000, -1.000000000000000000 ) ) ;
#2401 = CARTESIAN_POINT ( 'NONE',  ( -9.045553118584754415, -8.482981269326389295, 3.747395293195558847E-16 ) ) ;
#2402 = DIRECTION ( 'NONE',  ( -1.000000000000000000, 0.000000000000000000, -0.000000000000000000 ) ) ;
#2403 = CIRCLE ( 'NONE', #3971, 22.99899999999999878 ) ;
#2404 = DIRECTION ( 'NONE',  ( 1.000000000000000000, -0.000000000000000000, -0.000000000000000000 ) ) ;
#2405 = ORIENTED_EDGE ( 'NONE', *, *, #4443, .T. ) ;
#2406 = EDGE_CURVE ( 'NONE', #712, #2737, #1572, .T. ) ;
#2407 = AXIS2_PLACEMENT_3D ( 'NONE', #1034, #98, #3844 ) ;
#2408 = CARTESIAN_POINT ( 'NONE',  ( 0.000000000000000000, 0.000000000000000000, 0.000000000000000000 ) ) ;
#2409 = ORIENTED_EDGE ( 'NONE', *, *, #256, .F. ) ;
#2410 = VECTOR ( 'NONE', #6538, 1000.000000000000000 ) ;
#2411 = DIRECTION ( 'NONE',  ( 0.000000000000000000, 0.3090169943749479509, -0.9510565162951534202 ) ) ;
#2412 = CARTESIAN_POINT ( 'NONE',  ( 1.500000000000000444, 24.77821629063821973, -1.039229259764577140 ) ) ;
#2413 = CARTESIAN_POINT ( 'NONE',  ( -1.500000000000000222, 1.836970198721030181E-16, 0.000000000000000000 ) ) ;
#2414 = CARTESIAN_POINT ( 'NONE',  ( -6.661525743073271499, 1.789546221321743458, 10.00000000000000000 ) ) ;
#2415 = EDGE_CURVE ( 'NONE', #1082, #5236, #5720, .T. ) ;
#2416 = CARTESIAN_POINT ( 'NONE',  ( -0.3972327064967883237, 12.29993208790119930, 6.857782953271941950E-17 ) ) ;
#2417 = CYLINDRICAL_SURFACE ( 'NONE', #11947, 9.599999999999997868 ) ;
#2418 = LINE ( 'NONE', #9032, #1017 ) ;
#2419 = VERTEX_POINT ( 'NONE', #11986 ) ;
#2420 = EDGE_CURVE ( 'NONE', #4090, #4817, #3363, .T. ) ;
#2421 = ORIENTED_EDGE ( 'NONE', *, *, #5046, .F. ) ;
#2422 = CIRCLE ( 'NONE', #10241, 24.80000000000000071 ) ;
#2423 = ORIENTED_EDGE ( 'NONE', *, *, #6105, .F. ) ;
#2424 = CARTESIAN_POINT ( 'NONE',  ( -11.21689850596896676, 9.520844388990630236, 10.00000000000000000 ) ) ;
#2425 = CARTESIAN_POINT ( 'NONE',  ( 3.000000000000000888, 11.20082935824103387, -20.08719549084852929 ) ) ;
#2426 = DIRECTION ( 'NONE',  ( -1.000000000000000000, -0.000000000000000000, 0.000000000000000000 ) ) ;
#2427 = EDGE_CURVE ( 'NONE', #6354, #8063, #8137, .T. ) ;
#2428 = CIRCLE ( 'NONE', #2050, 3.000000000000000000 ) ;
#2429 = CARTESIAN_POINT ( 'NONE',  ( 6.563569809674826061, -3.208372544468511833, 3.747395293195558847E-16 ) ) ;
#2430 = CYLINDRICAL_SURFACE ( 'NONE', #6472, 9.599999999999997868 ) ;
#2431 = FACE_OUTER_BOUND ( 'NONE', #9331, .T. ) ;
#2432 = ORIENTED_EDGE ( 'NONE', *, *, #1003, .T. ) ;
#2433 = ORIENTED_EDGE ( 'NONE', *, *, #1414, .T. ) ;
#2434 = APPLICATION_PROTOCOL_DEFINITION ( 'draft international standard', 'automotive_design', 1998, #10992 ) ;
#2435 = CARTESIAN_POINT ( 'NONE',  ( 13.92981926110968161, -3.738495919395732781, 10.00000000000000000 ) ) ;
#2436 = ORIENTED_EDGE ( 'NONE', *, *, #11340, .F. ) ;
#2437 = CARTESIAN_POINT ( 'NONE',  ( 3.000000000000000888, -13.62355943574031869, 17.97274125076070206 ) ) ;
#2438 = AXIS2_PLACEMENT_3D ( 'NONE', #7154, #2519, #4545 ) ;
#2439 = LINE ( 'NONE', #8298, #7007 ) ;
#2440 = CARTESIAN_POINT ( 'NONE',  ( 0.000000000000000000, 16.45023496161686438, -15.42759117534368407 ) ) ;
#2441 = CARTESIAN_POINT ( 'NONE',  ( 3.000000000000000888, -22.15038895030651744, 4.240409074144028345 ) ) ;
#2442 = ORIENTED_EDGE ( 'NONE', *, *, #7387, .T. ) ;
#2443 = DIRECTION ( 'NONE',  ( -1.000000000000000000, -0.000000000000000000, 0.000000000000000000 ) ) ;
#2444 = DIRECTION ( 'NONE',  ( -1.000000000000000000, 0.000000000000000000, 0.000000000000000000 ) ) ;
#2445 = CARTESIAN_POINT ( 'NONE',  ( 9.774996403550728630, -5.644905071530503804, 6.857782953271941950E-17 ) ) ;
#2446 = CARTESIAN_POINT ( 'NONE',  ( 0.000000000000000000, -1.039229259764660407, 24.77821629063821263 ) ) ;
#2447 = EDGE_LOOP ( 'NONE', ( #7209, #1560, #7375, #3832 ) ) ;
#2448 = CARTESIAN_POINT ( 'NONE',  ( 3.000000000000000888, 0.000000000000000000, 0.000000000000000000 ) ) ;
#2449 = ORIENTED_EDGE ( 'NONE', *, *, #5083, .F. ) ;
#2450 = CARTESIAN_POINT ( 'NONE',  ( 10.00611923916671309, -2.842981073525690405, 10.00000000000000000 ) ) ;
#2451 = EDGE_LOOP ( 'NONE', ( #5692, #7493, #1820, #3021 ) ) ;
#2452 = LINE ( 'NONE', #3620, #5793 ) ;
#2453 = CIRCLE ( 'NONE', #7141, 22.99900000000000233 ) ;
#2454 = CARTESIAN_POINT ( 'NONE',  ( 0.000000000000000000, 12.88318129270205148, -18.51065745848364230 ) ) ;
#2455 = ORIENTED_EDGE ( 'NONE', *, *, #2734, .F. ) ;
#2456 = CARTESIAN_POINT ( 'NONE',  ( 19.00000000000000000, 0.000000000000000000, 0.000000000000000000 ) ) ;
#2457 = DIRECTION ( 'NONE',  ( 0.000000000000000000, 0.4067366430758009854, -0.9135454576426006446 ) ) ;
#2458 = CARTESIAN_POINT ( 'NONE',  ( 8.025946968469186871, -7.769110617520879281, 10.00000000000000000 ) ) ;
#2459 = CARTESIAN_POINT ( 'NONE',  ( 3.000000000000000888, 21.96011696265484403, 5.135568396240393518 ) ) ;
#2460 = CARTESIAN_POINT ( 'NONE',  ( 2.103398428914359020, -12.69820342197950680, 3.747395293195558847E-16 ) ) ;
#2461 = EDGE_CURVE ( 'NONE', #9359, #3469, #2553, .T. ) ;
#2462 = DIRECTION ( 'NONE',  ( 0.000000000000000000, 0.000000000000000000, 1.000000000000000000 ) ) ;
#2463 = ORIENTED_EDGE ( 'NONE', *, *, #10939, .F. ) ;
#2464 = CIRCLE ( 'NONE', #2864, 22.99899999999999523 ) ;
#2465 = EDGE_CURVE ( 'NONE', #7274, #2665, #9618, .T. ) ;
#2466 = EDGE_CURVE ( 'NONE', #10699, #9213, #10198, .T. ) ;
#2467 = DIRECTION ( 'NONE',  ( -1.000000000000000000, 0.000000000000000000, 0.000000000000000000 ) ) ;
#2468 = B_SPLINE_CURVE_WITH_KNOTS ( 'NONE', 3,
 ( #10420, #5834, #7664, #2039, #4850, #5779, #8591, #8698, #11497, #3119, #5938, #6779, #281, #10504, #9653, #9451, #4801, #7613, #1313, #6704, #7803, #5854, #147, #3217, #8611, #7868, #6881, #6935, #334, #10439, #1080, #10624, #9643, #11422, #6761, #4137, #1198, #10497, #9584, #4813, #273, #6817, #5049, #2057, #2982, #3043, #5795, #4015, #8550, #11538, #2113, #4873, #2174, #3893, #8788, #4937, #9520, #8673, #11357, #2235, #1262, #4994, #5972, #10556, #11601, #5740, #4072, #1137, #7741, #11478, #9701, #3098, #7685, #5916, #208, #393, #3957, #8732, #3162, #1997, #9463, #10806, #9757, #2536, #9884, #3334, #8044, #2351, #8165, #4434, #2416, #2292, #2478, #9999, #456, #3406, #6157, #3270, #6211, #6273, #4309, #7175, #9936, #8852, #5108, #1626, #5361, #7115, #11778, #6028, #1439, #9825, #4195, #3466, #1376, #7922, #10918, #4376, #10867, #8109, #11893, #9090, #11836, #1557, #699, #10680, #11654, #1497, #6992, #10739, #5229, #3521, #6092, #5293, #5172, #9030, #8908, #641, #514, #11712, #4249, #7976, #7053, #8962, #575, #757, #8227, #943, #6512, #8291, #7357, #5415, #7294, #1798, #12, #11168, #11101, #6340, #11231, #6450, #12017, #8414, #1861, #5596, #5469, #10246, #3764, #11952, #9386, #2718, #3582, #12073, #7486, #8483, #1920, #9327, #2843, #2781, #9142, #1681, #6568, #7419, #4679, #1009, #5537, #6391, #10302, #2605, #1733, #5656, #4493, #10062, #9203, #4622, #3641, #10115, #4743, #79, #7233, #10986, #11047, #10182, #2660, #822, #9267, #4559, #886, #8354 ),
 .UNSPECIFIED., .F., .F.,
 ( 4, 2, 2, 2, 2, 2, 2, 2, 2, 2, 2, 2, 2, 2, 2, 2, 2, 2, 2, 2, 2, 2, 2, 2, 2, 2, 2, 2, 2, 2, 2, 2, 2, 2, 2, 2, 2, 2, 2, 2, 2, 2, 2, 2, 2, 2, 2, 2, 2, 2, 2, 2, 2, 2, 2, 2, 2, 2, 2, 2, 2, 2, 2, 2, 2, 2, 2, 2, 2, 2, 2, 2, 2, 2, 2, 2, 2, 2, 2, 2, 2, 2, 2, 2, 2, 2, 2, 2, 2, 2, 2, 2, 2, 2, 2, 2, 2, 2, 2, 2, 2, 2, 2, 4 ),
 ( 0.000000000000000000, 0.007812500000000000000, 0.01562500000000000000, 0.02343750000000000000, 0.03125000000000000000, 0.03906250000000000000, 0.04687500000000000000, 0.05468750000000000000, 0.06250000000000000000, 0.07031250000000000000, 0.07812500000000000000, 0.08593750000000000000, 0.09375000000000000000, 0.1015624999999999861, 0.1093750000000000000, 0.1171875000000000000, 0.1250000000000000000, 0.1328125000000000000, 0.1406250000000000000, 0.1484375000000000000, 0.1562500000000000000, 0.1640624999999999722, 0.1718750000000000000, 0.1796875000000000000, 0.1875000000000000000, 0.1953125000000000000, 0.2031249999999999722, 0.2109375000000000000, 0.2187500000000000000, 0.2265625000000000000, 0.2343750000000000000, 0.2421875000000000000, 0.2500000000000000000, 0.2578125000000000000, 0.2656250000000000000, 0.2734375000000000000, 0.2812500000000000000, 0.2890625000000000000, 0.2968750000000000000, 0.3046875000000000000, 0.3125000000000000000, 0.3203125000000000000, 0.3281249999999999445, 0.3359375000000000000, 0.3437500000000000000, 0.3515625000000000000, 0.3593750000000000000, 0.3671874999999999445, 0.3750000000000000000, 0.3828125000000000000, 0.3906250000000000000, 0.3984375000000000000, 0.4062499999999999445, 0.4140625000000000000, 0.4218750000000000000, 0.4296875000000000000, 0.4375000000000000000, 0.4453125000000000000, 0.4531250000000000000, 0.4609375000000000000, 0.4687500000000000000, 0.4765625000000000000, 0.4843750000000000000, 0.4921875000000000000, 0.5000000000000000000, 0.5078125000000000000, 0.5156250000000000000, 0.5234375000000000000, 0.5312500000000000000, 0.5390625000000000000, 0.5468750000000000000, 0.5546875000000000000, 0.5625000000000000000, 0.5703125000000000000, 0.5781250000000000000, 0.5859375000000000000, 0.5937500000000000000, 0.6015625000000000000, 0.6093750000000000000, 0.6171874999999998890, 0.6250000000000000000, 0.6328125000000000000, 0.6406250000000000000, 0.6484375000000000000, 0.6562499999999998890, 0.6640625000000000000, 0.6718750000000000000, 0.6796875000000000000, 0.6875000000000000000, 0.6953124999999998890, 0.7031250000000000000, 0.7109375000000000000, 0.7187500000000000000, 0.7265625000000000000, 0.7343749999999998890, 0.7421875000000000000, 0.7500000000000000000, 0.7656250000000000000, 0.7812500000000000000, 0.7968750000000000000, 0.8124999999999998890, 0.8281250000000000000, 0.8437500000000000000, 0.8499999999999999778 ),
 .UNSPECIFIED. ) ;
#2469 = ORIENTED_EDGE ( 'NONE', *, *, #4802, .F. ) ;
#2470 = CARTESIAN_POINT ( 'NONE',  ( 0.000000000000000000, 0.000000000000000000, 0.000000000000000000 ) ) ;
#2471 = DIRECTION ( 'NONE',  ( 0.000000000000000000, -0.9510565162951566398, 0.3090169943749382919 ) ) ;
#2472 = VERTEX_POINT ( 'NONE', #5438 ) ;
#2473 = DIRECTION ( 'NONE',  ( 0.000000000000000000, 0.000000000000000000, 1.000000000000000000 ) ) ;
#2474 = CIRCLE ( 'NONE', #9317, 9.599999999999997868 ) ;
#2475 = CARTESIAN_POINT ( 'NONE',  ( 3.000000000000000888, 13.62355943574044481, -17.97274125076060258 ) ) ;
#2476 = LINE ( 'NONE', #6210, #1783 ) ;
#2477 = EDGE_CURVE ( 'NONE', #2132, #7388, #11759, .T. ) ;
#2478 = CARTESIAN_POINT ( 'NONE',  ( 2.578468386369129117, 11.91291369680096857, 6.857782953271941950E-17 ) ) ;
#2479 = DIRECTION ( 'NONE',  ( -1.000000000000000000, 0.000000000000000000, 0.000000000000000000 ) ) ;
#2480 = EDGE_CURVE ( 'NONE', #11249, #10264, #5905, .T. ) ;
#2481 = DIRECTION ( 'NONE',  ( -1.000000000000000000, -0.000000000000000000, 0.000000000000000000 ) ) ;
#2482 = ORIENTED_EDGE ( 'NONE', *, *, #11815, .F. ) ;
#2483 = ORIENTED_EDGE ( 'NONE', *, *, #5860, .T. ) ;
#2484 = ORIENTED_EDGE ( 'NONE', *, *, #901, .F. ) ;
#2485 = CARTESIAN_POINT ( 'NONE',  ( -9.680665087126289592, -7.686621967951973389, 10.00000000000000000 ) ) ;
#2486 = DIRECTION ( 'NONE',  ( -1.000000000000000000, 0.000000000000000000, 0.000000000000000000 ) ) ;
#2487 = CARTESIAN_POINT ( 'NONE',  ( 3.000000000000000888, 0.000000000000000000, 0.000000000000000000 ) ) ;
#2488 = CARTESIAN_POINT ( 'NONE',  ( -6.036922680726758195, -0.4347383792561972382, 3.747395293195558847E-16 ) ) ;
#2489 = AXIS2_PLACEMENT_3D ( 'NONE', #8607, #953, #11297 ) ;
#2490 = DIRECTION ( 'NONE',  ( -1.000000000000000000, -0.000000000000000000, -0.000000000000000000 ) ) ;
#2491 = CARTESIAN_POINT ( 'NONE',  ( 3.000000000000000888, -8.645255683529166291, 23.24434456306322261 ) ) ;
#2492 = ORIENTED_EDGE ( 'NONE', *, *, #9536, .F. ) ;
#2493 = ORIENTED_EDGE ( 'NONE', *, *, #7774, .T. ) ;
#2494 = ORIENTED_EDGE ( 'NONE', *, *, #8157, .T. ) ;
#2495 = LINE ( 'NONE', #1581, #10778 ) ;
#2496 = CARTESIAN_POINT ( 'NONE',  ( 0.000000000000000000, -13.62355943574031869, 17.97274125076070206 ) ) ;
#2497 = CARTESIAN_POINT ( 'NONE',  ( 0.000000000000000000, 0.000000000000000000, 0.000000000000000000 ) ) ;
#2498 = CIRCLE ( 'NONE', #1324, 9.599999999999997868 ) ;
#2499 = DIRECTION ( 'NONE',  ( 0.000000000000000000, 0.000000000000000000, 1.000000000000000000 ) ) ;
#2500 = ORIENTED_EDGE ( 'NONE', *, *, #10665, .T. ) ;
#2501 = ADVANCED_FACE ( 'NONE', ( #11073 ), #2573, .T. ) ;
#2502 = CARTESIAN_POINT ( 'NONE',  ( 3.000000000000000888, -22.54798042742717357, -0.4575788569254196636 ) ) ;
#2503 = LINE ( 'NONE', #9166, #1035 ) ;
#2504 = CARTESIAN_POINT ( 'NONE',  ( 2.084091085258986009, 8.931495281877380066, 6.857782953271941950E-17 ) ) ;
#2505 = CARTESIAN_POINT ( 'NONE',  ( 0.000000000000000000, 0.000000000000000000, 0.000000000000000000 ) ) ;
#2506 = AXIS2_PLACEMENT_3D ( 'NONE', #3532, #6166, #7125 ) ;
#2507 = AXIS2_PLACEMENT_3D ( 'NONE', #11053, #10008, #5371 ) ;
#2508 = CARTESIAN_POINT ( 'NONE',  ( 19.99999999999999645, 2.449293598294706119E-15, 20.00000000000000000 ) ) ;
#2509 = EDGE_CURVE ( 'NONE', #11319, #1445, #7458, .T. ) ;
#2510 = ORIENTED_EDGE ( 'NONE', *, *, #10571, .F. ) ;
#2511 = ORIENTED_EDGE ( 'NONE', *, *, #8650, .T. ) ;
#2512 = CARTESIAN_POINT ( 'NONE',  ( -6.012500708481080203, 0.06204199954272103523, 10.00000000000000000 ) ) ;
#2513 = ORIENTED_EDGE ( 'NONE', *, *, #9356, .T. ) ;
#2514 = LINE ( 'NONE', #11930, #6190 ) ;
#2515 = ORIENTED_EDGE ( 'NONE', *, *, #3657, .T. ) ;
#2516 = AXIS2_PLACEMENT_3D ( 'NONE', #2258, #11499, #10459 ) ;
#2517 = DIRECTION ( 'NONE',  ( 1.000000000000000000, 0.000000000000000000, 0.000000000000000000 ) ) ;
#2518 = VECTOR ( 'NONE', #4069, 1000.000000000000000 ) ;
#2519 = DIRECTION ( 'NONE',  ( -1.000000000000000000, 0.000000000000000000, 0.000000000000000000 ) ) ;
#2520 = CARTESIAN_POINT ( 'NONE',  ( 6.396238541183701720, 6.183590428399974748, 10.00000000000000000 ) ) ;
#2521 = CARTESIAN_POINT ( 'NONE',  ( -19.00000000000000000, 2.326828918379970970E-15, 0.000000000000000000 ) ) ;
#2522 = EDGE_CURVE ( 'NONE', #5068, #2284, #11352, .T. ) ;
#2523 = CARTESIAN_POINT ( 'NONE',  ( 3.000000000000000888, 22.15038895030654942, -4.240409074143872914 ) ) ;
#2524 = VERTEX_POINT ( 'NONE', #9357 ) ;
#2525 = DIRECTION ( 'NONE',  ( -1.000000000000000000, 0.000000000000000000, 0.000000000000000000 ) ) ;
#2526 = VERTEX_POINT ( 'NONE', #1654 ) ;
#2527 = AXIS2_PLACEMENT_3D ( 'NONE', #599, #3429, #2791 ) ;
#2528 = CARTESIAN_POINT ( 'NONE',  ( 4.525508228541170297, -0.2388087992699348128, 3.747395293195558847E-16 ) ) ;
#2529 = FACE_OUTER_BOUND ( 'NONE', #6695, .T. ) ;
#2530 = EDGE_LOOP ( 'NONE', ( #7673, #11425, #9407, #859 ) ) ;
#2531 = CARTESIAN_POINT ( 'NONE',  ( 0.000000000000000000, -2.811977935937640005, -22.37663021667346896 ) ) ;
#2532 = DIRECTION ( 'NONE',  ( -1.000000000000000000, -0.000000000000000000, 0.000000000000000000 ) ) ;
#2533 = CARTESIAN_POINT ( 'NONE',  ( 3.000000000000000888, -17.97274125076064877, -13.62355943574037731 ) ) ;
#2534 = CARTESIAN_POINT ( 'NONE',  ( 0.3111040546027374343, -4.780743156735979049, 10.00000000000000000 ) ) ;
#2535 = AXIS2_PLACEMENT_3D ( 'NONE', #600, #664, #4334 ) ;
#2536 = CARTESIAN_POINT ( 'NONE',  ( -9.546882484473291797, 8.373557015400844961, 6.857782953271941950E-17 ) ) ;
#2537 = CARTESIAN_POINT ( 'NONE',  ( 1.500000000000000444, -21.97817939804031795, -11.48910920600707009 ) ) ;
#2538 = AXIS2_PLACEMENT_3D ( 'NONE', #11261, #10510, #108 ) ;
#2539 = CARTESIAN_POINT ( 'NONE',  ( 3.000000000000000888, 15.40502424595171327, -19.43515443678387555 ) ) ;
#2540 = ORIENTED_EDGE ( 'NONE', *, *, #6499, .T. ) ;
#2541 = EDGE_LOOP ( 'NONE', ( #847, #6542, #9288, #5997 ) ) ;
#2542 = EDGE_LOOP ( 'NONE', ( #9524, #788, #830, #11863 ) ) ;
#2543 = AXIS2_PLACEMENT_3D ( 'NONE', #10742, #10002, #8965 ) ;
#2544 = PRODUCT_RELATED_PRODUCT_CATEGORY ( 'part', '', ( #220 ) ) ;
#2545 = CARTESIAN_POINT ( 'NONE',  ( 10.36190401371066727, -8.216093097539268086, 10.00000000000000000 ) ) ;
#2546 = EDGE_CURVE ( 'NONE', #5965, #9994, #10370, .T. ) ;
#2547 = AXIS2_PLACEMENT_3D ( 'NONE', #11291, #9455, #1073 ) ;
#2548 = CARTESIAN_POINT ( 'NONE',  ( 3.000000000000000888, 0.000000000000000000, 0.000000000000000000 ) ) ;
#2549 = CARTESIAN_POINT ( 'NONE',  ( -4.500000000000000888, -0.5000000000000000000, 3.000000000000000000 ) ) ;
#2550 = EDGE_CURVE ( 'NONE', #1912, #11191, #2954, .T. ) ;
#2551 = CARTESIAN_POINT ( 'NONE',  ( 6.411932913580776550, 4.469049885107575726, 3.747395293195558847E-16 ) ) ;
#2552 = DIRECTION ( 'NONE',  ( 0.000000000000000000, 0.1045284632676469622, 0.9945218953682738450 ) ) ;
#2553 = CIRCLE ( 'NONE', #9394, 9.599999999999997868 ) ;
#2554 = AXIS2_PLACEMENT_3D ( 'NONE', #10908, #2525, #11880 ) ;
#2555 = DIRECTION ( 'NONE',  ( -1.000000000000000000, 0.000000000000000000, 0.000000000000000000 ) ) ;
#2556 = ORIENTED_EDGE ( 'NONE', *, *, #4478, .T. ) ;
#2557 = VERTEX_POINT ( 'NONE', #11920 ) ;
#2558 = CONTEXT_DEPENDENT_SHAPE_REPRESENTATION ( #8656, #4147 ) ;
#2559 = EDGE_LOOP ( 'NONE', ( #1863, #1284, #11117, #1939 ) ) ;
#2560 = CARTESIAN_POINT ( 'NONE',  ( 3.000000000000000888, 21.14796121233196402, 9.039786367038912474 ) ) ;
#2561 = CARTESIAN_POINT ( 'NONE',  ( 0.000000000000000000, -20.41249101028205004, -9.589108953448107542 ) ) ;
#2562 = CIRCLE ( 'NONE', #4519, 9.599999999999996092 ) ;
#2563 = VECTOR ( 'NONE', #7503, 1000.000000000000000 ) ;
#2564 = UNCERTAINTY_MEASURE_WITH_UNIT (LENGTH_MEASURE( 1.000000000000000082E-05 ), #752, 'distance_accuracy_value', 'NONE');
#2565 = DIRECTION ( 'NONE',  ( -1.000000000000000000, -0.000000000000000000, -0.000000000000000000 ) ) ;
#2566 = ORIENTED_EDGE ( 'NONE', *, *, #6432, .F. ) ;
#2567 = VECTOR ( 'NONE', #4717, 1000.000000000000000 ) ;
#2568 = FACE_OUTER_BOUND ( 'NONE', #6706, .T. ) ;
#2569 = CARTESIAN_POINT ( 'NONE',  ( 0.000000000000000000, 0.000000000000000000, 0.000000000000000000 ) ) ;
#2570 = CARTESIAN_POINT ( 'NONE',  ( 0.3111040546027372677, -4.780743156735971944, 6.857782953271941950E-17 ) ) ;
#2571 = EDGE_CURVE ( 'NONE', #1140, #5646, #4510, .T. ) ;
#2572 = CIRCLE ( 'NONE', #414, 24.80000000000000071 ) ;
#2573 = CYLINDRICAL_SURFACE ( 'NONE', #2188, 9.599999999999997868 ) ;
#2574 = AXIS2_PLACEMENT_3D ( 'NONE', #2294, #4139, #3044 ) ;
#2575 = FACE_OUTER_BOUND ( 'NONE', #7463, .T. ) ;
#2576 = AXIS2_PLACEMENT_3D ( 'NONE', #1100, #6660, #6720 ) ;
#2577 = ORIENTED_EDGE ( 'NONE', *, *, #3677, .F. ) ;
#2578 = EDGE_CURVE ( 'NONE', #1648, #6277, #11927, .T. ) ;
#2579 = ORIENTED_EDGE ( 'NONE', *, *, #10478, .F. ) ;
#2580 = CARTESIAN_POINT ( 'NONE',  ( 7.527773320476329744, 0.8933511214756656438, 10.00000000000000000 ) ) ;
#2581 = DIRECTION ( 'NONE',  ( 0.000000000000000000, 0.9135454576426018658, -0.4067366430757979323 ) ) ;
#2582 = ORIENTED_EDGE ( 'NONE', *, *, #10346, .F. ) ;
#2583 = ORIENTED_EDGE ( 'NONE', *, *, #11480, .T. ) ;
#2584 = AXIS2_PLACEMENT_3D ( 'NONE', #12059, #2832, #6554 ) ;
#2585 = AXIS2_PLACEMENT_3D ( 'NONE', #8520, #1052, #119 ) ;
#2586 = DIRECTION ( 'NONE',  ( -1.000000000000000000, 0.000000000000000000, 0.000000000000000000 ) ) ;
#2587 = EDGE_CURVE ( 'NONE', #9333, #10794, #3551, .T. ) ;
#2588 = VECTOR ( 'NONE', #6003, 1000.000000000000000 ) ;
#2589 = CARTESIAN_POINT ( 'NONE',  ( 0.000000000000000000, 0.000000000000000000, 0.000000000000000000 ) ) ;
#2590 = CARTESIAN_POINT ( 'NONE',  ( 8.235329212248927888, -1.783486464602662691, 10.00000000000000000 ) ) ;
#2591 =( LENGTH_UNIT ( ) NAMED_UNIT ( * ) SI_UNIT ( .MILLI., .METRE. ) );
#2592 = CARTESIAN_POINT ( 'NONE',  ( 3.000000000000000888, 23.24434456306324748, 8.645255683529086355 ) ) ;
#2593 = ORIENTED_EDGE ( 'NONE', *, *, #1685, .F. ) ;
#2594 = DIRECTION ( 'NONE',  ( -1.000000000000000000, 0.000000000000000000, 0.000000000000000000 ) ) ;
#2595 = ORIENTED_EDGE ( 'NONE', *, *, #7737, .F. ) ;
#2596 = CIRCLE ( 'NONE', #48, 9.599999999999997868 ) ;
#2597 = CARTESIAN_POINT ( 'NONE',  ( -0.1881845630465192321, -6.755137126427047001, 3.747395293195558847E-16 ) ) ;
#2598 = CARTESIAN_POINT ( 'NONE',  ( 0.000000000000000000, -5.117118920208643118, 22.42251312757878168 ) ) ;
#2599 =( NAMED_UNIT ( * ) SI_UNIT ( $, .STERADIAN. ) SOLID_ANGLE_UNIT ( ) );
#2600 = ORIENTED_EDGE ( 'NONE', *, *, #4533, .T. ) ;
#2601 = CYLINDRICAL_SURFACE ( 'NONE', #11293, 24.80000000000000071 ) ;
#2602 = CARTESIAN_POINT ( 'NONE',  ( 3.000000000000000888, 0.000000000000000000, 0.000000000000000000 ) ) ;
#2603 = CARTESIAN_POINT ( 'NONE',  ( -0.8869411547437835441, -7.669649013129178350, 10.00000000000000000 ) ) ;
#2604 = AXIS2_PLACEMENT_3D ( 'NONE', #7142, #670, #1652 ) ;
#2605 = CARTESIAN_POINT ( 'NONE',  ( -4.006926059188537614, 5.225193401749451461, 6.857782953271941950E-17 ) ) ;
#2606 = FACE_OUTER_BOUND ( 'NONE', #11035, .T. ) ;
#2607 = CARTESIAN_POINT ( 'NONE',  ( 0.000000000000000000, 0.000000000000000000, 0.000000000000000000 ) ) ;
#2608 = AXIS2_PLACEMENT_3D ( 'NONE', #824, #7544, #4623 ) ;
#2609 = ORIENTED_EDGE ( 'NONE', *, *, #2320, .F. ) ;
#2610 = VERTEX_POINT ( 'NONE', #7325 ) ;
#2611 = CIRCLE ( 'NONE', #10025, 9.599999999999996092 ) ;
#2612 = CARTESIAN_POINT ( 'NONE',  ( 1.629745903656676820, 14.14889381255350287, 10.00000000000000000 ) ) ;
#2613 = DIRECTION ( 'NONE',  ( 0.000000000000000000, 0.000000000000000000, 1.000000000000000000 ) ) ;
#2614 = DIRECTION ( 'NONE',  ( 0.000000000000000000, 0.000000000000000000, 1.000000000000000000 ) ) ;
#2615 = CARTESIAN_POINT ( 'NONE',  ( 7.357672848543031385, 2.125097602832226151, 3.747395293195558847E-16 ) ) ;
#2616 = AXIS2_PLACEMENT_3D ( 'NONE', #9855, #6121, #3548 ) ;
#2617 = LINE ( 'NONE', #9896, #5894 ) ;
#2618 = ORIENTED_EDGE ( 'NONE', *, *, #9536, .T. ) ;
#2619 = EDGE_CURVE ( 'NONE', #3033, #4684, #6419, .T. ) ;
#2620 = DIRECTION ( 'NONE',  ( -1.000000000000000000, -0.000000000000000000, -0.000000000000000000 ) ) ;
#2621 = ORIENTED_EDGE ( 'NONE', *, *, #4113, .T. ) ;
#2622 = EDGE_CURVE ( 'NONE', #9863, #5773, #4119, .T. ) ;
#2623 = ORIENTED_EDGE ( 'NONE', *, *, #2619, .T. ) ;
#2624 = CARTESIAN_POINT ( 'NONE',  ( -3.432991321284830200, 4.402131891631372973, 10.00000000000000000 ) ) ;
#2625 = CARTESIAN_POINT ( 'NONE',  ( 3.000000000000000888, 0.000000000000000000, 0.000000000000000000 ) ) ;
#2626 = DIRECTION ( 'NONE',  ( 0.000000000000000000, 0.000000000000000000, 1.000000000000000000 ) ) ;
#2627 = CARTESIAN_POINT ( 'NONE',  ( 0.000000000000000000, 0.000000000000000000, 0.000000000000000000 ) ) ;
#2628 = CARTESIAN_POINT ( 'NONE',  ( 0.000000000000000000, 0.000000000000000000, 20.00000000000000000 ) ) ;
#2629 = CARTESIAN_POINT ( 'NONE',  ( -5.542557460684657045, -4.854674288179716690, 6.857782953271941950E-17 ) ) ;
#2630 = EDGE_CURVE ( 'NONE', #1468, #3303, #8690, .T. ) ;
#2631 = DIRECTION ( 'NONE',  ( -1.000000000000000000, 0.000000000000000000, 0.000000000000000000 ) ) ;
#2632 = AXIS2_PLACEMENT_3D ( 'NONE', #6862, #8946, #4180 ) ;
#2633 = ORIENTED_EDGE ( 'NONE', *, *, #7856, .F. ) ;
#2634 = LINE ( 'NONE', #10152, #8624 ) ;
#2635 = VERTEX_POINT ( 'NONE', #11434 ) ;
#2636 = ORIENTED_EDGE ( 'NONE', *, *, #1030, .T. ) ;
#2637 = CARTESIAN_POINT ( 'NONE',  ( -7.370305768634982435, 4.727533884956532262, 10.00000000000000000 ) ) ;
#2638 = ORIENTED_EDGE ( 'NONE', *, *, #6237, .T. ) ;
#2639 = EDGE_CURVE ( 'NONE', #5055, #2557, #6076, .T. ) ;
#2640 = DIRECTION ( 'NONE',  ( -1.000000000000000000, 0.000000000000000000, 0.000000000000000000 ) ) ;
#2641 = ORIENTED_EDGE ( 'NONE', *, *, #2825, .F. ) ;
#2642 = DIRECTION ( 'NONE',  ( 0.000000000000000000, -0.8090169943749406789, -0.5877852522924823520 ) ) ;
#2643 = CARTESIAN_POINT ( 'NONE',  ( 3.000000000000000888, 0.000000000000000000, 0.000000000000000000 ) ) ;
#2644 = CARTESIAN_POINT ( 'NONE',  ( 8.281812197879517612, -14.90260015151217488, 6.857782953271941950E-17 ) ) ;
#2645 = EDGE_CURVE ( 'NONE', #5516, #8218, #9196, .T. ) ;
#2646 = CARTESIAN_POINT ( 'NONE',  ( 3.000000000000000888, -0.4575788569253416149, 22.54798042742717712 ) ) ;
#2647 = DIRECTION ( 'NONE',  ( -1.000000000000000000, 0.000000000000000000, 0.000000000000000000 ) ) ;
#2648 = CARTESIAN_POINT ( 'NONE',  ( 0.000000000000000000, 24.77821629063821973, -1.039229259764575364 ) ) ;
#2649 = ORIENTED_EDGE ( 'NONE', *, *, #12031, .F. ) ;
#2650 = VECTOR ( 'NONE', #10799, 1000.000000000000000 ) ;
#2651 = CARTESIAN_POINT ( 'NONE',  ( 3.120778274233606098, -6.257845451233481349, 3.747395293195558847E-16 ) ) ;
#2652 = CARTESIAN_POINT ( 'NONE',  ( 1.500000000000000444, 13.28910708463157420, -20.93895013827567553 ) ) ;
#2653 = DIRECTION ( 'NONE',  ( 1.000000000000000000, 0.000000000000000000, 0.000000000000000000 ) ) ;
#2654 = DIRECTION ( 'NONE',  ( 0.000000000000000000, 0.000000000000000000, 1.000000000000000000 ) ) ;
#2655 = DIRECTION ( 'NONE',  ( 1.000000000000000000, 0.000000000000000000, 0.000000000000000000 ) ) ;
#2656 = DIRECTION ( 'NONE',  ( -1.000000000000000000, -0.000000000000000000, 0.000000000000000000 ) ) ;
#2657 = CARTESIAN_POINT ( 'NONE',  ( -15.18624859168667918, -5.715447929355455869, 10.00000000000000000 ) ) ;
#2658 = EDGE_CURVE ( 'NONE', #8897, #12050, #3929, .T. ) ;
#2659 = VECTOR ( 'NONE', #11814, 1000.000000000000000 ) ;
#2660 = CARTESIAN_POINT ( 'NONE',  ( 3.913389251770639010, -3.458713887698550593, 6.857782953271941950E-17 ) ) ;
#2661 = CARTESIAN_POINT ( 'NONE',  ( 0.000000000000000000, 0.4575788569251889593, 22.54798042742718067 ) ) ;
#2662 = CYLINDRICAL_SURFACE ( 'NONE', #6841, 9.599999999999997868 ) ;
#2663 = ORIENTED_EDGE ( 'NONE', *, *, #10393, .F. ) ;
#2664 = EDGE_CURVE ( 'NONE', #2526, #8541, #1951, .T. ) ;
#2665 = VERTEX_POINT ( 'NONE', #4713 ) ;
#2666 = VECTOR ( 'NONE', #1048, 1000.000000000000000 ) ;
#2667 = CARTESIAN_POINT ( 'NONE',  ( 11.72652038055310086, 7.297668919378235586, 10.00000000000000000 ) ) ;
#2668 = DIRECTION ( 'NONE',  ( 1.000000000000000000, 0.000000000000000000, 0.000000000000000000 ) ) ;
#2669 = CARTESIAN_POINT ( 'NONE',  ( 3.000000000000000888, 20.78471918669860941, 8.753070780933226658 ) ) ;
#2670 = CARTESIAN_POINT ( 'NONE',  ( 2.467392210070199710, 7.745125807189173095, 3.747395293195558847E-16 ) ) ;
#2671 = CARTESIAN_POINT ( 'NONE',  ( 1.445324715877976729, -3.701599742324197084, 3.747395293195558847E-16 ) ) ;
#2672 = FACE_OUTER_BOUND ( 'NONE', #4102, .T. ) ;
#2673 = DIRECTION ( 'NONE',  ( -1.000000000000000000, -0.000000000000000000, -0.000000000000000000 ) ) ;
#2674 = ORIENTED_EDGE ( 'NONE', *, *, #5866, .T. ) ;
#2675 = ORIENTED_EDGE ( 'NONE', *, *, #1223, .T. ) ;
#2676 = CYLINDRICAL_SURFACE ( 'NONE', #4956, 9.599999999999997868 ) ;
#2677 = FACE_OUTER_BOUND ( 'NONE', #8457, .T. ) ;
#2678 = AXIS2_PLACEMENT_3D ( 'NONE', #5922, #3397, #2242 ) ;
#2679 = SURFACE_SIDE_STYLE ('',( #5212 ) ) ;
#2680 = LINE ( 'NONE', #10945, #713 ) ;
#2681 = CARTESIAN_POINT ( 'NONE',  ( 0.000000000000000000, 0.000000000000000000, 0.000000000000000000 ) ) ;
#2682 = ADVANCED_FACE ( 'NONE', ( #4889 ), #8627, .T. ) ;
#2683 = CARTESIAN_POINT ( 'NONE',  ( 0.000000000000000000, 0.000000000000000000, 0.000000000000000000 ) ) ;
#2684 = CARTESIAN_POINT ( 'NONE',  ( -2.682496113117365244, -7.114254743909630641, 6.857782953271941950E-17 ) ) ;
#2685 = DIRECTION ( 'NONE',  ( 0.000000000000000000, 0.7431448254773954654, -0.6691306063588569053 ) ) ;
#2686 = ORIENTED_EDGE ( 'NONE', *, *, #1882, .T. ) ;
#2687 = ORIENTED_EDGE ( 'NONE', *, *, #9609, .T. ) ;
#2688 = CARTESIAN_POINT ( 'NONE',  ( 3.000000000000000888, -19.75591328264879110, -10.87771529938182091 ) ) ;
#2689 = ORIENTED_EDGE ( 'NONE', *, *, #2844, .F. ) ;
#2690 = VECTOR ( 'NONE', #4114, 1000.000000000000000 ) ;
#2691 = ORIENTED_EDGE ( 'NONE', *, *, #11991, .F. ) ;
#2692 = CARTESIAN_POINT ( 'NONE',  ( -5.315861670734006061, 2.363279591656077816, 10.00000000000000000 ) ) ;
#2693 = EDGE_CURVE ( 'NONE', #5571, #4684, #7997, .T. ) ;
#2694 = ORIENTED_EDGE ( 'NONE', *, *, #9281, .F. ) ;
#2695 = DIRECTION ( 'NONE',  ( -1.000000000000000000, 0.000000000000000000, -0.000000000000000000 ) ) ;
#2696 = ORIENTED_EDGE ( 'NONE', *, *, #11963, .F. ) ;
#2697 = ADVANCED_FACE ( 'NONE', ( #7517 ), #5809, .T. ) ;
#2698 = CARTESIAN_POINT ( 'NONE',  ( 0.000000000000000000, -15.80756504416678432, -19.10918332567973721 ) ) ;
#2699 = EDGE_CURVE ( 'NONE', #10972, #5532, #4484, .T. ) ;
#2700 = DIRECTION ( 'NONE',  ( -1.000000000000000000, -0.000000000000000000, -0.000000000000000000 ) ) ;
#2701 = CARTESIAN_POINT ( 'NONE',  ( -6.947552178111049415, -1.615339808524829168, 10.00000000000000000 ) ) ;
#2702 = AXIS2_PLACEMENT_3D ( 'NONE', #7626, #9413, #7568 ) ;
#2703 = DIRECTION ( 'NONE',  ( 0.000000000000000000, 0.000000000000000000, -1.000000000000000000 ) ) ;
#2704 = DIRECTION ( 'NONE',  ( 0.000000000000000000, 0.6691306063588593478, -0.7431448254773932449 ) ) ;
#2705 = EDGE_LOOP ( 'NONE', ( #3783, #7591, #7363, #126 ) ) ;
#2706 = CARTESIAN_POINT ( 'NONE',  ( 1.499999999999999556, 1.039229259764835600, -24.77821629063820907 ) ) ;
#2707 = ORIENTED_EDGE ( 'NONE', *, *, #10507, .F. ) ;
#2708 = CARTESIAN_POINT ( 'NONE',  ( -5.862605222286285667, -1.923479314576677535, 3.747395293195558847E-16 ) ) ;
#2709 = VECTOR ( 'NONE', #7824, 1000.000000000000000 ) ;
#2710 = CIRCLE ( 'NONE', #10129, 24.80000000000000071 ) ;
#2711 = DIRECTION ( 'NONE',  ( 0.000000000000000000, 0.000000000000000000, 1.000000000000000000 ) ) ;
#2712 =( NAMED_UNIT ( * ) PLANE_ANGLE_UNIT ( ) SI_UNIT ( $, .RADIAN. ) );
#2713 = ORIENTED_EDGE ( 'NONE', *, *, #7207, .F. ) ;
#2714 = CYLINDRICAL_SURFACE ( 'NONE', #8561, 22.99899999999999878 ) ;
#2715 = DIRECTION ( 'NONE',  ( 0.000000000000000000, 0.000000000000000000, -1.000000000000000000 ) ) ;
#2716 = DIRECTION ( 'NONE',  ( -1.000000000000000000, 0.000000000000000000, 0.000000000000000000 ) ) ;
#2717 = CYLINDRICAL_SURFACE ( 'NONE', #9212, 9.599999999999997868 ) ;
#2718 = CARTESIAN_POINT ( 'NONE',  ( -2.100379401128184664, -7.348625593045285065, 6.857782953271941950E-17 ) ) ;
#2719 = CARTESIAN_POINT ( 'NONE',  ( 3.000000000000000888, -24.53384959170460178, 3.623565124517029279 ) ) ;
#2720 = CIRCLE ( 'NONE', #8394, 22.99899999999999878 ) ;
#2721 = FACE_OUTER_BOUND ( 'NONE', #2447, .T. ) ;
#2722 = ORIENTED_EDGE ( 'NONE', *, *, #7395, .F. ) ;
#2723 = ORIENTED_EDGE ( 'NONE', *, *, #3657, .F. ) ;
#2724 = ORIENTED_EDGE ( 'NONE', *, *, #8230, .T. ) ;
#2725 = EDGE_CURVE ( 'NONE', #1706, #6294, #2126, .T. ) ;
#2726 = CARTESIAN_POINT ( 'NONE',  ( 3.000000000000000888, 0.000000000000000000, 0.000000000000000000 ) ) ;
#2727 = CARTESIAN_POINT ( 'NONE',  ( -7.370305768634982435, 4.727533884956532262, 10.00000000000000000 ) ) ;
#2728 = CIRCLE ( 'NONE', #8597, 9.599999999999997868 ) ;
#2729 = AXIS2_PLACEMENT_3D ( 'NONE', #10568, #3051, #8505 ) ;
#2730 = DIRECTION ( 'NONE',  ( -1.000000000000000000, -0.000000000000000000, -0.000000000000000000 ) ) ;
#2731 = CARTESIAN_POINT ( 'NONE',  ( 3.000000000000000888, 15.80756504416690866, 19.10918332567963418 ) ) ;
#2732 = CIRCLE ( 'NONE', #9573, 22.99899999999999523 ) ;
#2733 = CARTESIAN_POINT ( 'NONE',  ( 8.282588618525734248, 7.043362411858246297, 3.747395293195558847E-16 ) ) ;
#2734 = EDGE_CURVE ( 'NONE', #1630, #8186, #10547, .T. ) ;
#2735 = CARTESIAN_POINT ( 'NONE',  ( 4.321204520403003180, 2.017656881711011430, 3.747395293195558847E-16 ) ) ;
#2736 = CARTESIAN_POINT ( 'NONE',  ( 3.000000000000000888, 17.31945870441147406, 15.13242714128125499 ) ) ;
#2737 = VERTEX_POINT ( 'NONE', #1217 ) ;
#2738 = CIRCLE ( 'NONE', #3717, 22.99900000000000233 ) ;
#2739 = VERTEX_POINT ( 'NONE', #4827 ) ;
#2740 = LINE ( 'NONE', #10383, #1241 ) ;
#2741 = CARTESIAN_POINT ( 'NONE',  ( 1.500000000000000444, 6.668524164681940647, -23.88662356770108630 ) ) ;
#2742 = LINE ( 'NONE', #2931, #8579 ) ;
#2743 = AXIS2_PLACEMENT_3D ( 'NONE', #8356, #945, #3767 ) ;
#2744 = CARTESIAN_POINT ( 'NONE',  ( 3.000000000000000888, 20.78471918669872665, -8.753070780932940664 ) ) ;
#2745 = AXIS2_PLACEMENT_3D ( 'NONE', #1853, #8401, #5527 ) ;
#2746 = CARTESIAN_POINT ( 'NONE',  ( -11.08238827499517321, -10.71925978067678642, 3.747395293195558847E-16 ) ) ;
#2747 = CARTESIAN_POINT ( 'NONE',  ( -5.924299593718516554, 3.297400215539475710, 6.857782953271941950E-17 ) ) ;
#2748 = DIRECTION ( 'NONE',  ( 0.000000000000000000, 0.9135454576426018658, -0.4067366430757981544 ) ) ;
#2749 = VERTEX_POINT ( 'NONE', #3852 ) ;
#2750 = ORIENTED_EDGE ( 'NONE', *, *, #12034, .T. ) ;
#2751 = DIRECTION ( 'NONE',  ( 0.000000000000000000, 0.2079116908177532086, 0.9781476007338069101 ) ) ;
#2752 = VECTOR ( 'NONE', #3016, 1000.000000000000000 ) ;
#2753 = ORIENTED_EDGE ( 'NONE', *, *, #9125, .F. ) ;
#2754 = VERTEX_POINT ( 'NONE', #11314 ) ;
#2755 = CARTESIAN_POINT ( 'NONE',  ( -2.214925388402925410, 4.996014981202114846, 10.00000000000000000 ) ) ;
#2756 = AXIS2_PLACEMENT_3D ( 'NONE', #11332, #2956, #3075 ) ;
#2757 = DIRECTION ( 'NONE',  ( -0.000000000000000000, 1.000000000000000000, 0.000000000000000000 ) ) ;
#2758 = ORIENTED_EDGE ( 'NONE', *, *, #2263, .T. ) ;
#2759 = EDGE_CURVE ( 'NONE', #11368, #3881, #10741, .T. ) ;
#2760 = DIRECTION ( 'NONE',  ( -1.000000000000000000, -0.000000000000000000, -0.000000000000000000 ) ) ;
#2761 = CARTESIAN_POINT ( 'NONE',  ( 0.000000000000000000, 0.000000000000000000, 0.000000000000000000 ) ) ;
#2762 = CARTESIAN_POINT ( 'NONE',  ( 15.92723891616420673, -6.911623607273379655, 6.857782953271941950E-17 ) ) ;
#2763 = VECTOR ( 'NONE', #8595, 1000.000000000000000 ) ;
#2764 = CIRCLE ( 'NONE', #11551, 24.80000000000000071 ) ;
#2765 = AXIS2_PLACEMENT_3D ( 'NONE', #402, #3050, #11428 ) ;
#2766 = EDGE_CURVE ( 'NONE', #10279, #8218, #9379, .T. ) ;
#2767 = LINE ( 'NONE', #6495, #1002 ) ;
#2768 = ORIENTED_EDGE ( 'NONE', *, *, #1499, .F. ) ;
#2769 = ORIENTED_EDGE ( 'NONE', *, *, #8606, .T. ) ;
#2770 = CARTESIAN_POINT ( 'NONE',  ( 3.000000000000000888, 22.37663021667344054, -2.811977935937859385 ) ) ;
#2771 = EDGE_CURVE ( 'NONE', #8914, #1640, #4882, .T. ) ;
#2772 = ORIENTED_EDGE ( 'NONE', *, *, #6213, .T. ) ;
#2773 = ADVANCED_FACE ( 'NONE', ( #6657 ), #1042, .T. ) ;
#2774 = CARTESIAN_POINT ( 'NONE',  ( -0.4771094043438768861, 5.286185534804329400, 3.747395293195558847E-16 ) ) ;
#2775 = FACE_OUTER_BOUND ( 'NONE', #3857, .T. ) ;
#2776 = VERTEX_POINT ( 'NONE', #49 ) ;
#2777 = AXIS2_PLACEMENT_3D ( 'NONE', #8384, #3666, #1705 ) ;
#2778 = CARTESIAN_POINT ( 'NONE',  ( 3.000000000000000888, 0.3433949777331667397, 22.99643626497956816 ) ) ;
#2779 = CARTESIAN_POINT ( 'NONE',  ( 0.000000000000000000, 0.000000000000000000, 10.00000000000000000 ) ) ;
#2780 = CARTESIAN_POINT ( 'NONE',  ( 8.281812197879521165, -14.90260015151097228, 10.00000000000000000 ) ) ;
#2781 = CARTESIAN_POINT ( 'NONE',  ( -6.829322889802579510, -2.192323464439260849, 6.857782953271941950E-17 ) ) ;
#2782 = AXIS2_PLACEMENT_3D ( 'NONE', #9129, #7342, #741 ) ;
#2783 = EDGE_CURVE ( 'NONE', #9137, #1367, #577, .T. ) ;
#2784 = DIRECTION ( 'NONE',  ( -1.000000000000000000, 0.000000000000000000, -0.000000000000000000 ) ) ;
#2785 = AXIS2_PLACEMENT_3D ( 'NONE', #6493, #4781, #10408 ) ;
#2786 = ORIENTED_EDGE ( 'NONE', *, *, #3366, .F. ) ;
#2787 = AXIS2_PLACEMENT_3D ( 'NONE', #5978, #9707, #9591 ) ;
#2788 = APPLICATION_CONTEXT ( 'automotive_design' ) ;
#2789 = ORIENTED_EDGE ( 'NONE', *, *, #370, .T. ) ;
#2790 = VERTEX_POINT ( 'NONE', #2072 ) ;
#2791 = DIRECTION ( 'NONE',  ( 0.000000000000000000, 0.9135454576425990902, 0.4067366430758040385 ) ) ;
#2792 = CARTESIAN_POINT ( 'NONE',  ( -8.111627617515260624, 3.498804908652024093, 10.00000000000000000 ) ) ;
#2793 = CIRCLE ( 'NONE', #11777, 9.599999999999999645 ) ;
#2794 = DIRECTION ( 'NONE',  ( 0.000000000000000000, 0.3090169943749417336, 0.9510565162951555296 ) ) ;
#2795 = EDGE_CURVE ( 'NONE', #9064, #5856, #769, .T. ) ;
#2796 = LINE ( 'NONE', #5606, #6420 ) ;
#2797 = CARTESIAN_POINT ( 'NONE',  ( 2.257301671556970479, -9.631158585656898197, 3.747395293195558847E-16 ) ) ;
#2798 = CIRCLE ( 'NONE', #4757, 9.599999999999997868 ) ;
#2799 = LINE ( 'NONE', #5485, #1625 ) ;
#2800 = ADVANCED_FACE ( 'NONE', ( #9772 ), #6042, .T. ) ;
#2801 = CARTESIAN_POINT ( 'NONE',  ( 3.000000000000000888, 0.000000000000000000, 0.000000000000000000 ) ) ;
#2802 = VERTEX_POINT ( 'NONE', #8803 ) ;
#2803 = ORIENTED_EDGE ( 'NONE', *, *, #8473, .F. ) ;
#2804 = AXIS2_PLACEMENT_3D ( 'NONE', #6668, #1961, #1777 ) ;
#2805 = ORIENTED_EDGE ( 'NONE', *, *, #7362, .T. ) ;
#2806 = EDGE_LOOP ( 'NONE', ( #5585, #10926 ) ) ;
#2807 = CARTESIAN_POINT ( 'NONE',  ( 0.000000000000000000, 22.37663021667344054, 6.788022064062137595 ) ) ;
#2808 = VECTOR ( 'NONE', #3185, 1000.000000000000000 ) ;
#2809 = DIRECTION ( 'NONE',  ( 0.000000000000000000, 0.9510565162951523099, 0.3090169943749513370 ) ) ;
#2810 = EDGE_CURVE ( 'NONE', #4929, #5661, #4326, .T. ) ;
#2811 = DIRECTION ( 'NONE',  ( 0.000000000000000000, 0.4999999999999948375, 0.8660254037844415942 ) ) ;
#2812 = FACE_OUTER_BOUND ( 'NONE', #7133, .T. ) ;
#2813 = CIRCLE ( 'NONE', #66, 9.599999999999997868 ) ;
#2814 = CARTESIAN_POINT ( 'NONE',  ( 3.000000000000000888, 9.667200211210106531, -20.86861857134724474 ) ) ;
#2815 = CARTESIAN_POINT ( 'NONE',  ( 4.977139221860116258, 13.21892491369776934, 3.747395293195558847E-16 ) ) ;
#2816 = CARTESIAN_POINT ( 'NONE',  ( 2.529667540516381319, -4.392173529266732324, 6.857782953271941950E-17 ) ) ;
#2817 = DIRECTION ( 'NONE',  ( 1.000000000000000000, 0.000000000000000000, 0.000000000000000000 ) ) ;
#2818 = ORIENTED_EDGE ( 'NONE', *, *, #8790, .F. ) ;
#2819 = EDGE_LOOP ( 'NONE', ( #3914, #9286, #2148, #9287 ) ) ;
#2820 = DIRECTION ( 'NONE',  ( -1.000000000000000000, -0.000000000000000000, -0.000000000000000000 ) ) ;
#2821 = ORIENTED_EDGE ( 'NONE', *, *, #10767, .F. ) ;
#2822 = CIRCLE ( 'NONE', #2231, 22.99899999999999878 ) ;
#2823 = ORIENTED_EDGE ( 'NONE', *, *, #823, .F. ) ;
#2824 = LINE ( 'NONE', #4658, #3000 ) ;
#2825 = EDGE_CURVE ( 'NONE', #6662, #8629, #5074, .T. ) ;
#2826 = CARTESIAN_POINT ( 'NONE',  ( 3.000000000000000888, 0.000000000000000000, 0.000000000000000000 ) ) ;
#2827 = VERTEX_POINT ( 'NONE', #7938 ) ;
#2828 = CARTESIAN_POINT ( 'NONE',  ( 3.000000000000000888, -8.753070780933295936, 20.78471918669858098 ) ) ;
#2829 = DIRECTION ( 'NONE',  ( 0.000000000000000000, -0.6691306063588644548, 0.7431448254773885820 ) ) ;
#2830 = CARTESIAN_POINT ( 'NONE',  ( -2.100379401128186441, -7.348625593045292170, 10.00000000000000000 ) ) ;
#2831 = VECTOR ( 'NONE', #624, 1000.000000000000000 ) ;
#2832 = DIRECTION ( 'NONE',  ( -1.000000000000000000, 0.000000000000000000, 0.000000000000000000 ) ) ;
#2833 = FACE_OUTER_BOUND ( 'NONE', #9045, .T. ) ;
#2834 = VERTEX_POINT ( 'NONE', #5988 ) ;
#2835 = ORIENTED_EDGE ( 'NONE', *, *, #2699, .T. ) ;
#2836 = CARTESIAN_POINT ( 'NONE',  ( 3.000000000000000888, 21.97702544527767188, -6.779701584702504391 ) ) ;
#2837 = ORIENTED_EDGE ( 'NONE', *, *, #7522, .T. ) ;
#2838 = CARTESIAN_POINT ( 'NONE',  ( -9.470608727121586412, 11.15741021143934653, 10.00000000000000000 ) ) ;
#2839 = FACE_OUTER_BOUND ( 'NONE', #6431, .T. ) ;
#2840 = CARTESIAN_POINT ( 'NONE',  ( 3.000000000000000888, 8.753070780933430939, -20.78471918669851703 ) ) ;
#2841 = DIRECTION ( 'NONE',  ( 0.000000000000000000, 1.000000000000000000, 3.491481338843133355E-15 ) ) ;
#2842 = CARTESIAN_POINT ( 'NONE',  ( -15.59049818040342927, 3.373450308083567606, 10.00000000000000000 ) ) ;
#2844 = EDGE_CURVE ( 'NONE', #5571, #4018, #7606, .T. ) ;
#2843 = CARTESIAN_POINT ( 'NONE',  ( -6.451445390047170214, -3.308750875808896819, 6.857782953271941950E-17 ) ) ;
#2845 = DIRECTION ( 'NONE',  ( -1.000000000000000000, -0.000000000000000000, -0.000000000000000000 ) ) ;
#2846 = EDGE_CURVE ( 'NONE', #1751, #11132, #6253, .T. ) ;
#2847 = CARTESIAN_POINT ( 'NONE',  ( 0.000000000000000000, 22.42251312757886694, -5.117118920208269195 ) ) ;
#2848 = VERTEX_POINT ( 'NONE', #11793 ) ;
#2849 = AXIS2_PLACEMENT_3D ( 'NONE', #5223, #7863, #5103 ) ;
#2850 = ORIENTED_EDGE ( 'NONE', *, *, #7778, .F. ) ;
#2851 = ORIENTED_EDGE ( 'NONE', *, *, #5853, .T. ) ;
#2852 = CARTESIAN_POINT ( 'NONE',  ( 0.000000000000000000, 0.000000000000000000, 20.00000000000000000 ) ) ;
#2853 = CARTESIAN_POINT ( 'NONE',  ( 2.355103038863951781, 10.93470652055904146, 10.00000000000000000 ) ) ;
#2854 = EDGE_CURVE ( 'NONE', #8297, #3718, #5667, .T. ) ;
#2855 = DIRECTION ( 'NONE',  ( 0.000000000000000000, -0.6691306063588644548, 0.7431448254773886930 ) ) ;
#2856 = CYLINDRICAL_SURFACE ( 'NONE', #5640, 9.599999999999996092 ) ;
#2857 = ADVANCED_FACE ( 'NONE', ( #2431 ), #7129, .T. ) ;
#2858 = CARTESIAN_POINT ( 'NONE',  ( -3.516813791735896810, 7.717845097288992484, 3.747395293195558847E-16 ) ) ;
#2859 = DIRECTION ( 'NONE',  ( 1.000000000000000000, 0.000000000000000000, 0.000000000000000000 ) ) ;
#2860 = PLANE ( 'NONE',  #1202 ) ;
#2861 = ORIENTED_EDGE ( 'NONE', *, *, #3225, .T. ) ;
#2862 = EDGE_LOOP ( 'NONE', ( #6778, #7942 ) ) ;
#2863 = ORIENTED_EDGE ( 'NONE', *, *, #4074, .F. ) ;
#2864 = AXIS2_PLACEMENT_3D ( 'NONE', #4111, #3201, #433 ) ;
#2865 = VERTEX_POINT ( 'NONE', #8979 ) ;
#2866 = FACE_OUTER_BOUND ( 'NONE', #7146, .T. ) ;
#2867 = CARTESIAN_POINT ( 'NONE',  ( 0.000000000000000000, -8.753070780933015271, -20.78471918669869467 ) ) ;
#2868 = CARTESIAN_POINT ( 'NONE',  ( 3.000000000000000888, 23.05871956130134848, -9.128825345752797915 ) ) ;
#2869 = DIRECTION ( 'NONE',  ( -1.000000000000000000, 0.000000000000000000, -0.000000000000000000 ) ) ;
#2870 = CARTESIAN_POINT ( 'NONE',  ( 0.000000000000000000, 0.000000000000000000, 0.000000000000000000 ) ) ;
#2871 = VECTOR ( 'NONE', #9979, 1000.000000000000000 ) ;
#2872 = CARTESIAN_POINT ( 'NONE',  ( -13.25288834650809555, -7.646628085888695914, 3.747395293195558847E-16 ) ) ;
#2873 = CARTESIAN_POINT ( 'NONE',  ( 0.000000000000000000, -22.90635393027944744, -2.062268319295799568 ) ) ;
#2874 = CARTESIAN_POINT ( 'NONE',  ( 3.000000000000000888, 0.000000000000000000, 0.000000000000000000 ) ) ;
#2875 = DIRECTION ( 'NONE',  ( 0.000000000000000000, 0.000000000000000000, 1.000000000000000000 ) ) ;
#2876 = ORIENTED_EDGE ( 'NONE', *, *, #8305, .F. ) ;
#2877 = ORIENTED_EDGE ( 'NONE', *, *, #10619, .T. ) ;
#2878 = CARTESIAN_POINT ( 'NONE',  ( 3.000000000000000888, -15.13242714128131361, 17.31945870441142077 ) ) ;
#2879 = ORIENTED_EDGE ( 'NONE', *, *, #1828, .F. ) ;
#2880 = DIRECTION ( 'NONE',  ( -1.000000000000000000, 0.000000000000000000, -0.000000000000000000 ) ) ;
#2881 = EDGE_CURVE ( 'NONE', #3787, #67, #6108, .T. ) ;
#2882 = CYLINDRICAL_SURFACE ( 'NONE', #1302, 24.80000000000000071 ) ;
#2883 = ORIENTED_EDGE ( 'NONE', *, *, #6080, .T. ) ;
#2884 = DIRECTION ( 'NONE',  ( 1.000000000000000000, 0.000000000000000000, 0.000000000000000000 ) ) ;
#2885 = CARTESIAN_POINT ( 'NONE',  ( 3.000000000000000888, -0.3433949777330061459, -22.99643626497957172 ) ) ;
#2886 = CARTESIAN_POINT ( 'NONE',  ( 11.20109743375191691, 9.815261043521076090, 6.857782953271941950E-17 ) ) ;
#2887 = AXIS2_PLACEMENT_3D ( 'NONE', #9020, #4365, #11365 ) ;
#2888 = LINE ( 'NONE', #11274, #8823 ) ;
#2889 = ADVANCED_FACE ( 'NONE', ( #6895 ), #10881, .T. ) ;
#2890 = CARTESIAN_POINT ( 'NONE',  ( -10.00000000000000000, 0.000000000000000000, 0.000000000000000000 ) ) ;
#2891 = AXIS2_PLACEMENT_3D ( 'NONE', #4371, #11831, #7229 ) ;
#2892 = VERTEX_POINT ( 'NONE', #10639 ) ;
#2893 = VERTEX_POINT ( 'NONE', #8060 ) ;
#2894 = LINE ( 'NONE', #1059, #3144 ) ;
#2895 = VERTEX_POINT ( 'NONE', #2491 ) ;
#2896 = CARTESIAN_POINT ( 'NONE',  ( -10.19073739998278683, -11.62312336453203798, 10.00000000000000000 ) ) ;
#2897 = DIRECTION ( 'NONE',  ( -1.000000000000000000, 0.000000000000000000, 0.000000000000000000 ) ) ;
#2898 = SHAPE_REPRESENTATION_RELATIONSHIP ( 'NONE' , 'NONE' ,  #842, #323 ) ;
#2899 = AXIS2_PLACEMENT_3D ( 'NONE', #6860, #496, #8714 ) ;
#2900 = LINE ( 'NONE', #6623, #344 ) ;
#2901 = CARTESIAN_POINT ( 'NONE',  ( 1.500000000000000444, -11.48910920600699015, 21.97817939804034992 ) ) ;
#2902 = CARTESIAN_POINT ( 'NONE',  ( 1.748316258820582947, 15.14524454193559144, 10.00000000000000000 ) ) ;
#2903 = LINE ( 'NONE', #10485, #2374 ) ;
#2904 = CARTESIAN_POINT ( 'NONE',  ( 1.499999999999999556, -4.135161237383748301, 24.45282072769599679 ) ) ;
#2905 = DIRECTION ( 'NONE',  ( -1.000000000000000000, 0.000000000000000000, 0.000000000000000000 ) ) ;
#2906 = ORIENTED_EDGE ( 'NONE', *, *, #7311, .F. ) ;
#2907 = CARTESIAN_POINT ( 'NONE',  ( -5.000000000000000000, 0.000000000000000000, 0.000000000000000000 ) ) ;
#2908 = AXIS2_PLACEMENT_3D ( 'NONE', #5122, #4950, #1148 ) ;
#2909 = CIRCLE ( 'NONE', #10526, 24.80000000000000071 ) ;
#2910 = ORIENTED_EDGE ( 'NONE', *, *, #5420, .T. ) ;
#2911 = FACE_OUTER_BOUND ( 'NONE', #5246, .T. ) ;
#2912 = CARTESIAN_POINT ( 'NONE',  ( -1.719633853164447057, -9.543036404944420070, 10.00000000000000000 ) ) ;
#2913 = CARTESIAN_POINT ( 'NONE',  ( 3.000000000000000888, -11.20082935824089354, 20.08719549084861455 ) ) ;
#2914 = CARTESIAN_POINT ( 'NONE',  ( 10.51453309316909213, -0.3307463982597989571, 3.747395293195558847E-16 ) ) ;
#2915 = AXIS2_PLACEMENT_3D ( 'NONE', #8919, #8175, #7986 ) ;
#2916 = ADVANCED_FACE ( 'NONE', ( #9713 ), #7006, .T. ) ;
#2917 = CIRCLE ( 'NONE', #1345, 22.99899999999999523 ) ;
#2918 = CARTESIAN_POINT ( 'NONE',  ( 3.000000000000000888, -11.20082935824089354, 20.08719549084861455 ) ) ;
#2919 = EDGE_LOOP ( 'NONE', ( #7470, #11671, #9718, #3230 ) ) ;
#2920 = EDGE_CURVE ( 'NONE', #1233, #11333, #2732, .T. ) ;
#2921 = ORIENTED_EDGE ( 'NONE', *, *, #12072, .T. ) ;
#2922 = EDGE_CURVE ( 'NONE', #9017, #9796, #3229, .T. ) ;
#2923 = ORIENTED_EDGE ( 'NONE', *, *, #9421, .T. ) ;
#2924 = CARTESIAN_POINT ( 'NONE',  ( 0.000000000000000000, 0.000000000000000000, -15.00000000000000000 ) ) ;
#2925 = AXIS2_PLACEMENT_3D ( 'NONE', #2454, #9232, #3659 ) ;
#2926 = DIRECTION ( 'NONE',  ( 0.000000000000000000, 0.9135454576426019768, -0.4067366430757979878 ) ) ;
#2927 = EDGE_CURVE ( 'NONE', #11246, #531, #4289, .T. ) ;
#2928 = AXIS2_PLACEMENT_3D ( 'NONE', #7633, #4954, #7754 ) ;
#2929 = VERTEX_POINT ( 'NONE', #9659 ) ;
#2930 = DIRECTION ( 'NONE',  ( 1.000000000000000000, 0.000000000000000000, 0.000000000000000000 ) ) ;
#2931 = CARTESIAN_POINT ( 'NONE',  ( -7.228014483236704444E-17, 0.5000000000000005551, 0.000000000000000000 ) ) ;
#2932 = CARTESIAN_POINT ( 'NONE',  ( 0.000000000000000000, 0.000000000000000000, 4.000000000000000000 ) ) ;
#2933 = CARTESIAN_POINT ( 'NONE',  ( 2.103398428914359020, -12.69820342197950680, 3.747395293195558847E-16 ) ) ;
#2934 = DIRECTION ( 'NONE',  ( 0.000000000000000000, 0.000000000000000000, 1.000000000000000000 ) ) ;
#2935 = ORIENTED_EDGE ( 'NONE', *, *, #7095, .T. ) ;
#2936 = ORIENTED_EDGE ( 'NONE', *, *, #5921, .F. ) ;
#2937 = DIRECTION ( 'NONE',  ( -1.000000000000000000, 0.000000000000000000, 0.000000000000000000 ) ) ;
#2938 = ORIENTED_EDGE ( 'NONE', *, *, #11707, .T. ) ;
#2939 = DIRECTION ( 'NONE',  ( 1.000000000000000000, -0.000000000000000000, 0.000000000000000000 ) ) ;
#2940 = VECTOR ( 'NONE', #8167, 1000.000000000000000 ) ;
#2941 = ADVANCED_BREP_SHAPE_REPRESENTATION ( '', ( #4375, #8474 ), #5098 ) ;
#2942 = DIRECTION ( 'NONE',  ( 0.000000000000000000, -0.000000000000000000, 1.000000000000000000 ) ) ;
#2943 = VERTEX_POINT ( 'NONE', #9843 ) ;
#2944 = CIRCLE ( 'NONE', #6452, 24.80000000000000071 ) ;
#2945 = CARTESIAN_POINT ( 'NONE',  ( 0.000000000000000000, -24.53384959170460178, 3.623565124517029279 ) ) ;
#2946 = EDGE_CURVE ( 'NONE', #2802, #12019, #10148, .T. ) ;
#2947 = DIRECTION ( 'NONE',  ( -1.000000000000000000, -0.000000000000000000, -0.000000000000000000 ) ) ;
#2948 = CARTESIAN_POINT ( 'NONE',  ( 14.53830338343599848, -0.2437330612273620467, 6.857782953271941950E-17 ) ) ;
#2949 = FACE_OUTER_BOUND ( 'NONE', #8368, .T. ) ;
#2950 = CIRCLE ( 'NONE', #11350, 22.99899999999999878 ) ;
#2951 = EDGE_CURVE ( 'NONE', #2739, #2827, #3353, .T. ) ;
#2952 = CARTESIAN_POINT ( 'NONE',  ( 0.000000000000000000, 0.000000000000000000, -15.00000000000000000 ) ) ;
#2953 = ORIENTED_EDGE ( 'NONE', *, *, #4211, .F. ) ;
#2954 = CIRCLE ( 'NONE', #9782, 22.99899999999999878 ) ;
#2955 = EDGE_LOOP ( 'NONE', ( #11604, #11561, #1097, #11687 ) ) ;
#2956 = DIRECTION ( 'NONE',  ( -1.000000000000000000, -0.000000000000000000, 0.000000000000000000 ) ) ;
#2957 = ORIENTED_EDGE ( 'NONE', *, *, #2951, .T. ) ;
#2958 = AXIS2_PLACEMENT_3D ( 'NONE', #5748, #11366, #2988 ) ;
#2959 = MECHANICAL_DESIGN_GEOMETRIC_PRESENTATION_REPRESENTATION (  '', ( #799 ), #197 ) ;
#2960 = CARTESIAN_POINT ( 'NONE',  ( 13.68367311611256909, -8.822018488634764566, 10.00000000000000000 ) ) ;
#2961 = FACE_OUTER_BOUND ( 'NONE', #1577, .T. ) ;
#2962 = EDGE_CURVE ( 'NONE', #3365, #6277, #7188, .T. ) ;
#2964 = AXIS2_PLACEMENT_3D ( 'NONE', #8180, #3596, #11968 ) ;
#2963 = CYLINDRICAL_SURFACE ( 'NONE', #4842, 24.80000000000000071 ) ;
#2965 = VECTOR ( 'NONE', #3374, 1000.000000000000000 ) ;
#2966 = FACE_OUTER_BOUND ( 'NONE', #9587, .T. ) ;
#2967 = CARTESIAN_POINT ( 'NONE',  ( -11.61414229320030778, -6.453515506896109422, 10.00000000000000000 ) ) ;
#2968 = DIRECTION ( 'NONE',  ( 0.000000000000000000, 0.000000000000000000, 1.000000000000000000 ) ) ;
#2969 = CARTESIAN_POINT ( 'NONE',  ( 0.000000000000000000, 0.000000000000000000, 0.000000000000000000 ) ) ;
#2970 = PLANE ( 'NONE',  #10560 ) ;
#2971 = ORIENTED_EDGE ( 'NONE', *, *, #9082, .T. ) ;
#2972 = DIRECTION ( 'NONE',  ( -1.000000000000000000, -0.000000000000000000, -0.000000000000000000 ) ) ;
#2973 = CIRCLE ( 'NONE', #10786, 24.80000000000000071 ) ;
#2974 = AXIS2_PLACEMENT_3D ( 'NONE', #9143, #6275, #8963 ) ;
#2975 = VERTEX_POINT ( 'NONE', #11849 ) ;
#2976 = DIRECTION ( 'NONE',  ( 0.000000000000000000, 0.000000000000000000, 1.000000000000000000 ) ) ;
#2977 = CARTESIAN_POINT ( 'NONE',  ( -4.158289900078591117, 7.437556212722741478, 10.00000000000000000 ) ) ;
#2978 = DIRECTION ( 'NONE',  ( -1.000000000000000000, 0.000000000000000000, 0.000000000000000000 ) ) ;
#2979 = AXIS2_PLACEMENT_3D ( 'NONE', #11697, #5156, #9870 ) ;
#2980 = CARTESIAN_POINT ( 'NONE',  ( -9.820986981723351050, 1.626514086989862662, 10.00000000000000000 ) ) ;
#2981 = CIRCLE ( 'NONE', #3178, 24.80000000000000071 ) ;
#2982 = CARTESIAN_POINT ( 'NONE',  ( 8.547432504762587868, 12.33942397201039753, 6.857782953271941950E-17 ) ) ;
#2983 = CARTESIAN_POINT ( 'NONE',  ( 3.000000000000000888, 22.47229024614977533, 1.901833551798334909 ) ) ;
#2984 = VERTEX_POINT ( 'NONE', #9044 ) ;
#2985 = ORIENTED_EDGE ( 'NONE', *, *, #8756, .T. ) ;
#2986 = CYLINDRICAL_SURFACE ( 'NONE', #6402, 24.80000000000000071 ) ;
#2987 = CIRCLE ( 'NONE', #4946, 9.599999999999996092 ) ;
#2988 = DIRECTION ( 'NONE',  ( 0.000000000000000000, 0.000000000000000000, 1.000000000000000000 ) ) ;
#2989 = ORIENTED_EDGE ( 'NONE', *, *, #2946, .T. ) ;
#2990 = DIRECTION ( 'NONE',  ( -1.000000000000000000, 0.000000000000000000, 0.000000000000000000 ) ) ;
#2991 = CARTESIAN_POINT ( 'NONE',  ( 3.000000000000000888, -4.445336973061013275, 22.56530478845647991 ) ) ;
#2992 = DIRECTION ( 'NONE',  ( -1.000000000000000000, 0.000000000000000000, 0.000000000000000000 ) ) ;
#2993 = EDGE_CURVE ( 'NONE', #8735, #2776, #3712, .T. ) ;
#2994 = CARTESIAN_POINT ( 'NONE',  ( 9.683839015878911383, 10.01260560230520547, 3.747395293195558847E-16 ) ) ;
#2995 = CIRCLE ( 'NONE', #4174, 9.599999999999997868 ) ;
#2996 = EDGE_CURVE ( 'NONE', #3964, #2005, #9155, .T. ) ;
#2997 = CARTESIAN_POINT ( 'NONE',  ( 3.000000000000000888, 0.000000000000000000, 0.000000000000000000 ) ) ;
#2998 = ORIENTED_EDGE ( 'NONE', *, *, #1492, .T. ) ;
#2999 = ORIENTED_EDGE ( 'NONE', *, *, #2881, .T. ) ;
#3000 = VECTOR ( 'NONE', #1047, 1000.000000000000000 ) ;
#3001 = DIRECTION ( 'NONE',  ( 0.000000000000000000, 0.000000000000000000, 1.000000000000000000 ) ) ;
#3002 = CARTESIAN_POINT ( 'NONE',  ( 3.017784444055084947, -16.62017357425736463, 10.00000000000000000 ) ) ;
#3003 = VERTEX_POINT ( 'NONE', #137 ) ;
#3004 = LINE ( 'NONE', #11619, #12087 ) ;
#3005 = CARTESIAN_POINT ( 'NONE',  ( 1.500000000000000444, 9.128825345753341480, -23.05871956130112821 ) ) ;
#3006 = CIRCLE ( 'NONE', #6130, 9.599999999999997868 ) ;
#3007 = CARTESIAN_POINT ( 'NONE',  ( 3.000000000000000888, -20.78471918669866270, 8.753070780933086326 ) ) ;
#3008 = ORIENTED_EDGE ( 'NONE', *, *, #8254, .F. ) ;
#3009 = EDGE_CURVE ( 'NONE', #2790, #9956, #9102, .T. ) ;
#3010 = CARTESIAN_POINT ( 'NONE',  ( 3.000000000000000888, 4.240409074144393387, -22.15038895030644639 ) ) ;
#3011 = EDGE_CURVE ( 'NONE', #7440, #4186, #7224, .T. ) ;
#3012 = FACE_OUTER_BOUND ( 'NONE', #4439, .T. ) ;
#3013 = CARTESIAN_POINT ( 'NONE',  ( -1.124919223378054722, -13.71093750358708085, 6.857782953271941950E-17 ) ) ;
#3014 = DIRECTION ( 'NONE',  ( -1.000000000000000000, 0.000000000000000000, 0.000000000000000000 ) ) ;
#3015 = ORIENTED_EDGE ( 'NONE', *, *, #2466, .T. ) ;
#3016 = DIRECTION ( 'NONE',  ( -1.000000000000000000, -0.000000000000000000, 0.000000000000000000 ) ) ;
#3017 = CIRCLE ( 'NONE', #9263, 9.599999999999997868 ) ;
#3018 = EDGE_LOOP ( 'NONE', ( #2883, #11867 ) ) ;
#3019 = VERTEX_POINT ( 'NONE', #5376 ) ;
#3020 = DIRECTION ( 'NONE',  ( -1.000000000000000000, 0.000000000000000000, 0.000000000000000000 ) ) ;
#3021 = ORIENTED_EDGE ( 'NONE', *, *, #2250, .T. ) ;
#3022 = EDGE_CURVE ( 'NONE', #5920, #5848, #8609, .T. ) ;
#3023 = CARTESIAN_POINT ( 'NONE',  ( 12.25096627321952170, 6.291700371256734314, 10.00000000000000000 ) ) ;
#3024 = DIRECTION ( 'NONE',  ( 0.000000000000000000, -0.9781476007338034684, -0.2079116908177699174 ) ) ;
#3025 = ORIENTED_EDGE ( 'NONE', *, *, #11966, .F. ) ;
#3026 = DIRECTION ( 'NONE',  ( -1.000000000000000000, 0.000000000000000000, 0.000000000000000000 ) ) ;
#3027 = ADVANCED_FACE ( 'NONE', ( #8487 ), #4512, .T. ) ;
#3028 = DIRECTION ( 'NONE',  ( 0.000000000000000000, 0.000000000000000000, 1.000000000000000000 ) ) ;
#3029 = CARTESIAN_POINT ( 'NONE',  ( 8.588976300537440878, -11.19439025337201343, 10.00000000000000000 ) ) ;
#3030 = DIRECTION ( 'NONE',  ( -1.000000000000000000, 0.000000000000000000, 0.000000000000000000 ) ) ;
#3031 = CARTESIAN_POINT ( 'NONE',  ( -8.499083411061073789, 11.86528080735276269, 3.747395293195558847E-16 ) ) ;
#3032 = DIRECTION ( 'NONE',  ( 1.000000000000000000, 0.000000000000000000, 0.000000000000000000 ) ) ;
#3033 = VERTEX_POINT ( 'NONE', #1575 ) ;
#3034 = DIRECTION ( 'NONE',  ( -1.000000000000000000, 0.000000000000000000, 0.000000000000000000 ) ) ;
#3035 = AXIS2_PLACEMENT_3D ( 'NONE', #2589, #9252, #3385 ) ;
#3036 = ORIENTED_EDGE ( 'NONE', *, *, #6940, .F. ) ;
#3037 = ORIENTED_EDGE ( 'NONE', *, *, #114, .F. ) ;
#3038 = LINE ( 'NONE', #2167, #4652 ) ;
#3039 = CARTESIAN_POINT ( 'NONE',  ( -5.862605222286289219, -1.923479314576678423, 10.00000000000000000 ) ) ;
#3040 = EDGE_CURVE ( 'NONE', #3003, #2082, #12116, .T. ) ;
#3041 = CARTESIAN_POINT ( 'NONE',  ( -11.50000000000000178, 0.000000000000000000, 3.000000000000000000 ) ) ;
#3042 = CARTESIAN_POINT ( 'NONE',  ( 4.764169229607557732, 7.652272242165495619, 10.00000000000000000 ) ) ;
#3043 = CARTESIAN_POINT ( 'NONE',  ( 10.38524206949620243, 10.73010674553377264, 6.857782953271941950E-17 ) ) ;
#3044 = DIRECTION ( 'NONE',  ( -1.000000000000000000, 0.000000000000000000, 0.000000000000000000 ) ) ;
#3045 = ORIENTED_EDGE ( 'NONE', *, *, #1115, .F. ) ;
#3046 = ADVANCED_FACE ( 'NONE', ( #6353 ), #3538, .T. ) ;
#3047 = ORIENTED_EDGE ( 'NONE', *, *, #5684, .T. ) ;
#3048 = FACE_OUTER_BOUND ( 'NONE', #5578, .T. ) ;
#3049 = CIRCLE ( 'NONE', #301, 9.599999999999997868 ) ;
#3050 = DIRECTION ( 'NONE',  ( -1.000000000000000000, -0.000000000000000000, -0.000000000000000000 ) ) ;
#3051 = DIRECTION ( 'NONE',  ( -1.000000000000000000, -0.000000000000000000, -0.000000000000000000 ) ) ;
#3052 = DIRECTION ( 'NONE',  ( 1.000000000000000000, 0.000000000000000000, 0.000000000000000000 ) ) ;
#3053 = CARTESIAN_POINT ( 'NONE',  ( 7.078846155421574693, 8.354583459611243157, 3.747395293195558847E-16 ) ) ;
#3054 = AXIS2_PLACEMENT_3D ( 'NONE', #620, #4352, #8270 ) ;
#3055 = DIRECTION ( 'NONE',  ( 1.000000000000000000, 0.000000000000000000, 0.000000000000000000 ) ) ;
#3056 = VERTEX_POINT ( 'NONE', #1696 ) ;
#3057 = ORIENTED_EDGE ( 'NONE', *, *, #1238, .F. ) ;
#3058 = DIRECTION ( 'NONE',  ( 1.000000000000000000, 0.000000000000000000, 0.000000000000000000 ) ) ;
#3059 = CARTESIAN_POINT ( 'NONE',  ( -10.00000000000000000, 0.000000000000000000, 0.000000000000000000 ) ) ;
#3060 = VERTEX_POINT ( 'NONE', #2907 ) ;
#3061 = CARTESIAN_POINT ( 'NONE',  ( 3.000000000000000888, 1.039229259764488544, 24.77821629063822328 ) ) ;
#3062 = DIRECTION ( 'NONE',  ( -0.000000000000000000, -0.000000000000000000, -1.000000000000000000 ) ) ;
#3063 = DIRECTION ( 'NONE',  ( -1.000000000000000000, -0.000000000000000000, 0.000000000000000000 ) ) ;
#3064 = AXIS2_PLACEMENT_3D ( 'NONE', #3007, #1842, #10461 ) ;
#3065 = ORIENTED_EDGE ( 'NONE', *, *, #1526, .T. ) ;
#3066 = EDGE_CURVE ( 'NONE', #3787, #3750, #7421, .T. ) ;
#3067 = CARTESIAN_POINT ( 'NONE',  ( 3.000000000000000888, 17.31945870441167301, -15.13242714128102406 ) ) ;
#3068 = DIRECTION ( 'NONE',  ( -1.000000000000000000, -0.000000000000000000, -0.000000000000000000 ) ) ;
#3069 = CARTESIAN_POINT ( 'NONE',  ( -9.783806739528728258, -9.162509837619118969, 6.857782953271941950E-17 ) ) ;
#3070 = EDGE_CURVE ( 'NONE', #8369, #11808, #6408, .T. ) ;
#3071 = LINE ( 'NONE', #4207, #3766 ) ;
#3072 = ORIENTED_EDGE ( 'NONE', *, *, #11884, .T. ) ;
#3073 = CYLINDRICAL_SURFACE ( 'NONE', #4313, 4.000000000000000000 ) ;
#3074 = ORIENTED_EDGE ( 'NONE', *, *, #6475, .T. ) ;
#3075 = DIRECTION ( 'NONE',  ( 0.000000000000000000, -0.9781476007338034684, -0.2079116908177697509 ) ) ;
#3076 = VERTEX_POINT ( 'NONE', #8182 ) ;
#3077 = EDGE_CURVE ( 'NONE', #11191, #5192, #3882, .T. ) ;
#3078 = CARTESIAN_POINT ( 'NONE',  ( 10.36190401371066727, -8.216093097539268086, 10.00000000000000000 ) ) ;
#3079 = EDGE_CURVE ( 'NONE', #2393, #4550, #8416, .T. ) ;
#3080 = CARTESIAN_POINT ( 'NONE',  ( 0.000000000000000000, 7.402892494506579268, -21.30300407174355115 ) ) ;
#3081 = ADVANCED_FACE ( 'NONE', ( #4448 ), #9224, .T. ) ;
#3082 = ORIENTED_EDGE ( 'NONE', *, *, #6465, .F. ) ;
#3083 = CYLINDRICAL_SURFACE ( 'NONE', #11489, 22.99899999999999878 ) ;
#3084 = CARTESIAN_POINT ( 'NONE',  ( 0.000000000000000000, 0.000000000000000000, -5.000000000000000000 ) ) ;
#3085 = CARTESIAN_POINT ( 'NONE',  ( 11.40744677810891083, -1.317628706759891966, 10.00000000000000000 ) ) ;
#3086 = FACE_OUTER_BOUND ( 'NONE', #11136, .T. ) ;
#3087 = CARTESIAN_POINT ( 'NONE',  ( -12.61273389267802436, -8.731886703669292871, 3.747395293195558847E-16 ) ) ;
#3088 = CARTESIAN_POINT ( 'NONE',  ( 3.500000000000000000, 0.000000000000000000, -15.00000000000000000 ) ) ;
#3089 = CARTESIAN_POINT ( 'NONE',  ( 3.000000000000000888, 16.45023496161686438, -15.42759117534368407 ) ) ;
#3090 = EDGE_LOOP ( 'NONE', ( #4394, #8170, #6767, #5287 ) ) ;
#3091 = ORIENTED_EDGE ( 'NONE', *, *, #9839, .F. ) ;
#3092 = AXIS2_PLACEMENT_3D ( 'NONE', #12069, #4675, #3695 ) ;
#3093 = DIRECTION ( 'NONE',  ( -1.000000000000000000, 0.000000000000000000, 0.000000000000000000 ) ) ;
#3094 = CARTESIAN_POINT ( 'NONE',  ( 6.411932913581408044, 4.469049885107577502, 10.00000000000000000 ) ) ;
#3095 = DIRECTION ( 'NONE',  ( -1.000000000000000000, -0.000000000000000000, -0.000000000000000000 ) ) ;
#3096 = CARTESIAN_POINT ( 'NONE',  ( 0.000000000000000000, 4.445336973061169594, -22.56530478845644438 ) ) ;
#3097 = CARTESIAN_POINT ( 'NONE',  ( 9.774996403550735735, -5.644905071530105900, 10.00000000000000000 ) ) ;
#3098 = CARTESIAN_POINT ( 'NONE',  ( -9.783806739528728258, -9.162509837619118969, 6.857782953271941950E-17 ) ) ;
#3099 = DIRECTION ( 'NONE',  ( 0.000000000000000000, 0.000000000000000000, 1.000000000000000000 ) ) ;
#3100 = CIRCLE ( 'NONE', #9543, 9.599999999999996092 ) ;
#3101 = CARTESIAN_POINT ( 'NONE',  ( 0.000000000000000000, 7.402892494506291499, 21.30300407174365063 ) ) ;
#3102 = ORIENTED_EDGE ( 'NONE', *, *, #1127, .T. ) ;
#3103 = CIRCLE ( 'NONE', #8177, 1.500000000000000222 ) ;
#3104 = EDGE_CURVE ( 'NONE', #7905, #2021, #84, .T. ) ;
#3105 = ORIENTED_EDGE ( 'NONE', *, *, #8115, .F. ) ;
#3106 = CARTESIAN_POINT ( 'NONE',  ( 0.000000000000000000, 21.58580335785676496, 6.532525787311040943 ) ) ;
#3107 = CARTESIAN_POINT ( 'NONE',  ( 15.00667705184754119, -6.512453894250635145, 10.00000000000000000 ) ) ;
#3108 = VECTOR ( 'NONE', #4214, 1000.000000000000000 ) ;
#3109 = DIRECTION ( 'NONE',  ( -1.000000000000000000, 0.000000000000000000, 0.000000000000000000 ) ) ;
#3110 = CYLINDRICAL_SURFACE ( 'NONE', #7783, 18.49999999999999645 ) ;
#3111 = AXIS2_PLACEMENT_3D ( 'NONE', #3267, #3158, #6876 ) ;
#3112 = EDGE_CURVE ( 'NONE', #4077, #2329, #7817, .T. ) ;
#3113 = CARTESIAN_POINT ( 'NONE',  ( -11.62103867303406624, 2.700230667072888835, 3.747395293195558847E-16 ) ) ;
#3114 = DIRECTION ( 'NONE',  ( 0.000000000000000000, 0.000000000000000000, -1.000000000000000000 ) ) ;
#3115 = ORIENTED_EDGE ( 'NONE', *, *, #2795, .T. ) ;
#3116 = ORIENTED_EDGE ( 'NONE', *, *, #4369, .F. ) ;
#3117 = CARTESIAN_POINT ( 'NONE',  ( 13.67726327739690184, -10.50289975150004018, 10.00000000000000000 ) ) ;
#3118 = EDGE_LOOP ( 'NONE', ( #10774, #3702, #10024, #902 ) ) ;
#3119 = CARTESIAN_POINT ( 'NONE',  ( 8.281812197879517612, -14.90260015151217488, 6.857782953271941950E-17 ) ) ;
#3120 = CARTESIAN_POINT ( 'NONE',  ( 3.000000000000000888, -0.4575788569250363036, -22.54798042742718778 ) ) ;
#3121 = CARTESIAN_POINT ( 'NONE',  ( 0.000000000000000000, 0.000000000000000000, 4.000000000000000000 ) ) ;
#3122 = DIRECTION ( 'NONE',  ( 1.000000000000000000, 0.000000000000000000, 0.000000000000000000 ) ) ;
#3123 = ORIENTED_EDGE ( 'NONE', *, *, #4897, .F. ) ;
#3124 = CIRCLE ( 'NONE', #7411, 22.00000000000000000 ) ;
#3125 = AXIS2_PLACEMENT_3D ( 'NONE', #10449, #2066, #283 ) ;
#3126 = FACE_OUTER_BOUND ( 'NONE', #9611, .T. ) ;
#3127 = DIRECTION ( 'NONE',  ( 0.000000000000000000, 0.000000000000000000, -1.000000000000000000 ) ) ;
#3128 = CARTESIAN_POINT ( 'NONE',  ( -12.06849956494802889, -5.462025159506374017, 6.857782953271941950E-17 ) ) ;
#3129 = ORIENTED_EDGE ( 'NONE', *, *, #4791, .F. ) ;
#3130 = DIRECTION ( 'NONE',  ( -1.000000000000000000, 0.000000000000000000, 0.000000000000000000 ) ) ;
#3131 = DIRECTION ( 'NONE',  ( 1.000000000000000000, 0.000000000000000000, 0.000000000000000000 ) ) ;
#3132 = CIRCLE ( 'NONE', #2543, 22.99900000000000233 ) ;
#3133 = ORIENTED_EDGE ( 'NONE', *, *, #15, .F. ) ;
#3134 = CARTESIAN_POINT ( 'NONE',  ( 8.429646098664189680, -5.822225404888640377, 10.00000000000000000 ) ) ;
#3135 = DIRECTION ( 'NONE',  ( 1.000000000000000000, 0.000000000000000000, 0.000000000000000000 ) ) ;
#3136 = CARTESIAN_POINT ( 'NONE',  ( 3.000000000000000888, 22.90635393027949007, -2.062268319295327057 ) ) ;
#3137 = CARTESIAN_POINT ( 'NONE',  ( 3.000000000000000888, -10.87771529938174808, 19.75591328264882662 ) ) ;
#3138 = CARTESIAN_POINT ( 'NONE',  ( 13.99323099383125069, 4.495563823643928814, 10.00000000000000000 ) ) ;
#3139 = VECTOR ( 'NONE', #3262, 1000.000000000000000 ) ;
#3140 = CYLINDRICAL_SURFACE ( 'NONE', #10977, 9.599999999999997868 ) ;
#3141 = CIRCLE ( 'NONE', #1793, 22.99900000000000233 ) ;
#3142 = DIRECTION ( 'NONE',  ( 0.000000000000000000, 0.4067366430757948792, 0.9135454576426033091 ) ) ;
#3143 = EDGE_CURVE ( 'NONE', #8458, #2310, #11336, .T. ) ;
#3144 = VECTOR ( 'NONE', #8213, 1000.000000000000000 ) ;
#3145 = DIRECTION ( 'NONE',  ( -1.000000000000000000, 0.000000000000000000, 0.000000000000000000 ) ) ;
#3146 =( GEOMETRIC_REPRESENTATION_CONTEXT ( 3 ) GLOBAL_UNCERTAINTY_ASSIGNED_CONTEXT ( ( #10648 ) ) GLOBAL_UNIT_ASSIGNED_CONTEXT ( ( #1065, #10240, #5651 ) ) REPRESENTATION_CONTEXT ( 'NONE', 'WORKASPACE' ) );
#3147 = ORIENTED_EDGE ( 'NONE', *, *, #11513, .F. ) ;
#3148 = EDGE_CURVE ( 'NONE', #916, #4929, #9765, .T. ) ;
#3149 = DIRECTION ( 'NONE',  ( 0.000000000000000000, 0.000000000000000000, 1.000000000000000000 ) ) ;
#3150 = ORIENTED_EDGE ( 'NONE', *, *, #9355, .F. ) ;
#3151 = ORIENTED_EDGE ( 'NONE', *, *, #3784, .T. ) ;
#3152 = ORIENTED_EDGE ( 'NONE', *, *, #5032, .F. ) ;
#3153 = AXIS2_PLACEMENT_3D ( 'NONE', #1169, #248, #11453 ) ;
#3154 = VECTOR ( 'NONE', #3479, 1000.000000000000000 ) ;
#3155 = DIRECTION ( 'NONE',  ( -1.000000000000000000, 0.000000000000000000, 0.000000000000000000 ) ) ;
#3156 = CARTESIAN_POINT ( 'NONE',  ( -5.315861670734006061, 2.363279591656077816, 10.00000000000000000 ) ) ;
#3157 = AXIS2_PLACEMENT_3D ( 'NONE', #2688, #12049, #3669 ) ;
#3158 = DIRECTION ( 'NONE',  ( -0.000000000000000000, 0.000000000000000000, 1.000000000000000000 ) ) ;
#3159 = PRESENTATION_STYLE_ASSIGNMENT (( #8338 ) ) ;
#3160 = CARTESIAN_POINT ( 'NONE',  ( -1.916691774771272172, -10.52688368019216725, 10.00000000000000000 ) ) ;
#3161 = EDGE_CURVE ( 'NONE', #2212, #7191, #6867, .T. ) ;
#3162 = CARTESIAN_POINT ( 'NONE',  ( -12.98359546555289334, 0.8565524458115012507, 6.857782953271941950E-17 ) ) ;
#3163 = CARTESIAN_POINT ( 'NONE',  ( -11.50000000000000178, 0.000000000000000000, 4.000000000000000000 ) ) ;
#3164 = CARTESIAN_POINT ( 'NONE',  ( 3.000000000000000888, 0.000000000000000000, 0.000000000000000000 ) ) ;
#3165 = VECTOR ( 'NONE', #9887, 1000.000000000000000 ) ;
#3166 = VERTEX_POINT ( 'NONE', #9572 ) ;
#3167 = ORIENTED_EDGE ( 'NONE', *, *, #1272, .T. ) ;
#3168 = DIRECTION ( 'NONE',  ( -1.000000000000000000, 0.000000000000000000, 0.000000000000000000 ) ) ;
#3169 = EDGE_CURVE ( 'NONE', #3019, #2610, #2343, .T. ) ;
#3170 = CARTESIAN_POINT ( 'NONE',  ( 10.01890055165175042, -12.63311126014650121, 10.00000000000000000 ) ) ;
#3171 = PRODUCT_DEFINITION_SHAPE ( 'NONE', 'NONE',  #9054 ) ;
#3172 = DIRECTION ( 'NONE',  ( 0.000000000000000000, 0.000000000000000000, 1.000000000000000000 ) ) ;
#3173 = AXIS2_PLACEMENT_3D ( 'NONE', #1347, #10655, #7026 ) ;
#3174 = EDGE_CURVE ( 'NONE', #6126, #1881, #5675, .T. ) ;
#3175 = CARTESIAN_POINT ( 'NONE',  ( -8.694522232909450921, -2.966707450564700199, 3.747395293195558847E-16 ) ) ;
#3176 = DIRECTION ( 'NONE',  ( 0.000000000000000000, 0.000000000000000000, 1.000000000000000000 ) ) ;
#3177 = ORIENTED_EDGE ( 'NONE', *, *, #11615, .T. ) ;
#3178 = AXIS2_PLACEMENT_3D ( 'NONE', #8006, #11860, #11745 ) ;
#3179 = ORIENTED_EDGE ( 'NONE', *, *, #6335, .F. ) ;
#3180 = DIRECTION ( 'NONE',  ( 0.000000000000000000, 0.000000000000000000, 1.000000000000000000 ) ) ;
#3181 = CARTESIAN_POINT ( 'NONE',  ( -2.240087900411203758, -13.53314956822678639, 10.00000000000000000 ) ) ;
#3182 = EDGE_CURVE ( 'NONE', #6885, #9763, #3529, .T. ) ;
#3183 = VERTEX_POINT ( 'NONE', #9746 ) ;
#3184 = CARTESIAN_POINT ( 'NONE',  ( 3.000000000000000888, -16.45023496161675780, 15.42759117534379953 ) ) ;
#3185 = DIRECTION ( 'NONE',  ( -1.000000000000000000, 0.000000000000000000, 0.000000000000000000 ) ) ;
#3186 = DIRECTION ( 'NONE',  ( 0.000000000000000000, 0.000000000000000000, 1.000000000000000000 ) ) ;
#3187 = VERTEX_POINT ( 'NONE', #1128 ) ;
#3188 = COLOUR_RGB ( '', 0.72549020, 0.75294118, 0.79215686) ;
#3189 = DIRECTION ( 'NONE',  ( -1.000000000000000000, -0.000000000000000000, 0.000000000000000000 ) ) ;
#3190 = CYLINDRICAL_SURFACE ( 'NONE', #7662, 9.599999999999997868 ) ;
#3191 = CARTESIAN_POINT ( 'NONE',  ( 11.37845468071831512, 2.456417158213069829, 6.857782953271941950E-17 ) ) ;
#3192 = CIRCLE ( 'NONE', #10020, 22.99899999999999523 ) ;
#3193 = CARTESIAN_POINT ( 'NONE',  ( 0.000000000000000000, -22.37663021667341923, -2.811977935938010376 ) ) ;
#3194 = ORIENTED_EDGE ( 'NONE', *, *, #4791, .T. ) ;
#3195 = EDGE_CURVE ( 'NONE', #2893, #1721, #10362, .T. ) ;
#3196 = CARTESIAN_POINT ( 'NONE',  ( -20.00000000000000000, 2.449293598294706513E-15, -5.000000000000000000 ) ) ;
#3197 = ADVANCED_FACE ( 'NONE', ( #4860 ), #1365, .T. ) ;
#3198 = ORIENTED_EDGE ( 'NONE', *, *, #11230, .T. ) ;
#3199 = AXIS2_PLACEMENT_3D ( 'NONE', #1105, #11169, #6492 ) ;
#3200 = CARTESIAN_POINT ( 'NONE',  ( 4.889075487038677004, 9.929493272051477248, 10.00000000000000000 ) ) ;
#3201 = DIRECTION ( 'NONE',  ( -1.000000000000000000, -0.000000000000000000, 0.000000000000000000 ) ) ;
#3202 = DIRECTION ( 'NONE',  ( 0.000000000000000000, -0.1045284632676607151, 0.9945218953682726237 ) ) ;
#3203 = DIRECTION ( 'NONE',  ( -1.000000000000000000, 0.000000000000000000, -0.000000000000000000 ) ) ;
#3204 = CARTESIAN_POINT ( 'NONE',  ( 8.547432504761534489, 12.33942397201040286, 10.00000000000000000 ) ) ;
#3205 = DIRECTION ( 'NONE',  ( -1.000000000000000000, 0.000000000000000000, -0.000000000000000000 ) ) ;
#3206 = LINE ( 'NONE', #2046, #6892 ) ;
#3207 = DIRECTION ( 'NONE',  ( -1.000000000000000000, 0.000000000000000000, -0.000000000000000000 ) ) ;
#3208 = EDGE_LOOP ( 'NONE', ( #9036, #11751, #11869, #2989 ) ) ;
#3209 = CARTESIAN_POINT ( 'NONE',  ( 0.000000000000000000, 20.08719549084865008, 11.20082935824082249 ) ) ;
#3210 = ORIENTED_EDGE ( 'NONE', *, *, #7311, .T. ) ;
#3211 = CIRCLE ( 'NONE', #6345, 9.599999999999997868 ) ;
#3212 = CARTESIAN_POINT ( 'NONE',  ( 3.000000000000000888, -20.65684170206499815, 13.72351598154890873 ) ) ;
#3213 = DIRECTION ( 'NONE',  ( -1.000000000000000000, 0.000000000000000000, 0.000000000000000000 ) ) ;
#3214 = EDGE_CURVE ( 'NONE', #6896, #1851, #5086, .T. ) ;
#3215 = CARTESIAN_POINT ( 'NONE',  ( 0.000000000000000000, 16.85990652506920995, -15.64281154287580655 ) ) ;
#3216 = CARTESIAN_POINT ( 'NONE',  ( 0.6097887191948987429, 9.229167205757272896, 10.00000000000000000 ) ) ;
#3217 = CARTESIAN_POINT ( 'NONE',  ( -15.18624859168667562, -5.715447929355453205, 6.857782953271941950E-17 ) ) ;
#3218 = FACE_OUTER_BOUND ( 'NONE', #8138, .T. ) ;
#3219 = CIRCLE ( 'NONE', #8101, 22.99900000000000233 ) ;
#3220 = DIRECTION ( 'NONE',  ( 0.000000000000000000, 0.000000000000000000, 1.000000000000000000 ) ) ;
#3221 = VERTEX_POINT ( 'NONE', #7674 ) ;
#3222 = EDGE_LOOP ( 'NONE', ( #4062, #1669, #3129, #10941 ) ) ;
#3223 = EDGE_CURVE ( 'NONE', #3003, #9318, #4125, .T. ) ;
#3224 = FACE_OUTER_BOUND ( 'NONE', #9802, .T. ) ;
#3225 = EDGE_CURVE ( 'NONE', #9776, #2419, #6057, .T. ) ;
#3226 = CARTESIAN_POINT ( 'NONE',  ( 3.000000000000000888, 11.02759168516745270, 22.21333432029567945 ) ) ;
#3227 = CARTESIAN_POINT ( 'NONE',  ( 3.000000000000000888, -9.589108953447752270, -20.41249101028221702 ) ) ;
#3228 = CARTESIAN_POINT ( 'NONE',  ( 8.282588618525734248, 7.043362411858246297, 3.747395293195558847E-16 ) ) ;
#3229 = LINE ( 'NONE', #10753, #3313 ) ;
#3230 = ORIENTED_EDGE ( 'NONE', *, *, #9191, .T. ) ;
#3231 = ORIENTED_EDGE ( 'NONE', *, *, #338, .T. ) ;
#3232 = AXIS2_PLACEMENT_3D ( 'NONE', #10434, #9515, #1132 ) ;
#3233 = CARTESIAN_POINT ( 'NONE',  ( 14.54887842078032989, 0.9530482589066729959, 10.00000000000000000 ) ) ;
#3234 = VERTEX_POINT ( 'NONE', #4986 ) ;
#3235 = DIRECTION ( 'NONE',  ( -1.000000000000000000, 0.000000000000000000, -0.000000000000000000 ) ) ;
#3236 = DIRECTION ( 'NONE',  ( -1.000000000000000000, 0.000000000000000000, 0.000000000000000000 ) ) ;
#3237 = CARTESIAN_POINT ( 'NONE',  ( 0.000000000000000000, -9.128825345753185161, 23.05871956130119571 ) ) ;
#3238 = ORIENTED_EDGE ( 'NONE', *, *, #9057, .T. ) ;
#3239 = DIRECTION ( 'NONE',  ( 0.000000000000000000, 0.8660254037844363761, 0.5000000000000039968 ) ) ;
#3240 = AXIS2_PLACEMENT_3D ( 'NONE', #733, #7273, #10900 ) ;
#3241 = CARTESIAN_POINT ( 'NONE',  ( 3.000000000000000888, 22.99643626497956816, -0.3433949777332470088 ) ) ;
#3242 = CARTESIAN_POINT ( 'NONE',  ( -0.3972327064967883237, 12.29993208790119930, 6.857782953271941950E-17 ) ) ;
#3243 = ORIENTED_EDGE ( 'NONE', *, *, #8781, .T. ) ;
#3244 =( REPRESENTATION_RELATIONSHIP ('NONE','NONE', #8743, #5127 ) REPRESENTATION_RELATIONSHIP_WITH_TRANSFORMATION ( #8127 )SHAPE_REPRESENTATION_RELATIONSHIP( ) );
#3245 = LINE ( 'NONE', #4225, #2588 ) ;
#3246 = DIRECTION ( 'NONE',  ( 0.000000000000000000, 0.000000000000000000, 1.000000000000000000 ) ) ;
#3247 = ORIENTED_EDGE ( 'NONE', *, *, #8564, .T. ) ;
#3248 = EDGE_CURVE ( 'NONE', #8050, #1912, #11144, .T. ) ;
#3249 = AXIS2_PLACEMENT_3D ( 'NONE', #6957, #11675, #4035 ) ;
#3250 = CARTESIAN_POINT ( 'NONE',  ( -8.962830026514758686, 0.7152994853347287574, 10.00000000000000000 ) ) ;
#3251 = ORIENTED_EDGE ( 'NONE', *, *, #590, .T. ) ;
#3252 = FACE_OUTER_BOUND ( 'NONE', #4890, .T. ) ;
#3253 = PRESENTATION_STYLE_ASSIGNMENT (( #434 ) ) ;
#3254 = VERTEX_POINT ( 'NONE', #6807 ) ;
#3255 = DIRECTION ( 'NONE',  ( -1.000000000000000000, -0.000000000000000000, 0.000000000000000000 ) ) ;
#3256 = EDGE_CURVE ( 'NONE', #10797, #12019, #1373, .T. ) ;
#3257 = CARTESIAN_POINT ( 'NONE',  ( 3.000000000000000888, -18.40266524480597710, 13.79477846460790147 ) ) ;
#3258 = CARTESIAN_POINT ( 'NONE',  ( -4.625218816435448410, 8.325684435358759572, 10.00000000000000000 ) ) ;
#3259 = AXIS2_PLACEMENT_3D ( 'NONE', #4456, #2626, #7318 ) ;
#3260 = CARTESIAN_POINT ( 'NONE',  ( 0.000000000000000000, 22.54798042742718067, 9.142421143074731305 ) ) ;
#3261 = CARTESIAN_POINT ( 'NONE',  ( -5.008276813248563997, -11.55791719732261313, 3.747395293195558847E-16 ) ) ;
#3262 = DIRECTION ( 'NONE',  ( -1.000000000000000000, 0.000000000000000000, -0.000000000000000000 ) ) ;
#3263 = DIRECTION ( 'NONE',  ( 0.000000000000000000, 0.000000000000000000, -1.000000000000000000 ) ) ;
#3264 = ORIENTED_EDGE ( 'NONE', *, *, #3419, .F. ) ;
#3265 = CIRCLE ( 'NONE', #2678, 9.599999999999997868 ) ;
#3266 = FACE_OUTER_BOUND ( 'NONE', #1599, .T. ) ;
#3267 = CARTESIAN_POINT ( 'NONE',  ( 0.000000000000000000, 0.000000000000000000, 3.000000000000000000 ) ) ;
#3268 = CARTESIAN_POINT ( 'NONE',  ( 3.000000000000000888, 11.79560690673899970, -19.74380051311527495 ) ) ;
#3269 = CARTESIAN_POINT ( 'NONE',  ( -6.947552178111049415, -1.615339808524829168, 10.00000000000000000 ) ) ;
#3270 = CARTESIAN_POINT ( 'NONE',  ( 9.056240860197961595, 7.682302481599242228, 6.857782953271941950E-17 ) ) ;
#3271 = CYLINDRICAL_SURFACE ( 'NONE', #4733, 9.599999999999997868 ) ;
#3272 = CARTESIAN_POINT ( 'NONE',  ( 3.000000000000000888, 0.000000000000000000, 0.000000000000000000 ) ) ;
#3273 = VERTEX_POINT ( 'NONE', #3209 ) ;
#3274 = AXIS2_PLACEMENT_3D ( 'NONE', #1119, #1858, #940 ) ;
#3275 = ORIENTED_EDGE ( 'NONE', *, *, #2509, .F. ) ;
#3276 = ORIENTED_EDGE ( 'NONE', *, *, #5053, .F. ) ;
#3277 = CARTESIAN_POINT ( 'NONE',  ( -1.036640877615905287, -15.73686152240404823, 10.00000000000000000 ) ) ;
#3278 = ADVANCED_FACE ( 'NONE', ( #6753 ), #2164, .T. ) ;
#3279 = DIRECTION ( 'NONE',  ( 0.000000000000000000, 0.000000000000000000, 1.000000000000000000 ) ) ;
#3280 = CARTESIAN_POINT ( 'NONE',  ( 0.000000000000000000, 0.000000000000000000, 0.000000000000000000 ) ) ;
#3281 = VECTOR ( 'NONE', #6415, 1000.000000000000000 ) ;
#3282 = CARTESIAN_POINT ( 'NONE',  ( 5.319643049700911952, -8.526005966358411570, 3.747395293195558847E-16 ) ) ;
#3283 = CYLINDRICAL_SURFACE ( 'NONE', #6490, 24.80000000000000071 ) ;
#3284 = ADVANCED_FACE ( 'NONE', ( #10673 ), #8722, .T. ) ;
#3285 = CARTESIAN_POINT ( 'NONE',  ( 1.500000000000000444, 17.71842311621530186, 17.35216073792446423 ) ) ;
#3286 = VERTEX_POINT ( 'NONE', #9633 ) ;
#3287 = EDGE_LOOP ( 'NONE', ( #6319, #3619, #6295, #2432 ) ) ;
#3288 = CARTESIAN_POINT ( 'NONE',  ( -6.266017822847497420, 10.86399168115691438, 10.00000000000000000 ) ) ;
#3289 = EDGE_CURVE ( 'NONE', #10186, #9734, #2944, .T. ) ;
#3290 = ORIENTED_EDGE ( 'NONE', *, *, #6642, .T. ) ;
#3291 = CIRCLE ( 'NONE', #7785, 9.599999999999997868 ) ;
#3292 = CARTESIAN_POINT ( 'NONE',  ( 3.000000000000000888, 17.06259499759964271, -14.74749645579993995 ) ) ;
#3293 = CARTESIAN_POINT ( 'NONE',  ( 3.000000000000000888, 21.14796121233196402, 9.039786367038912474 ) ) ;
#3294 = PRODUCT_DEFINITION_CONTEXT ( 'detailed design', #6150, 'design' ) ;
#3295 = CARTESIAN_POINT ( 'NONE',  ( 3.000000000000000888, 2.745295967525994918, 22.83456483164690098 ) ) ;
#3296 = VERTEX_POINT ( 'NONE', #322 ) ;
#3297 = DIRECTION ( 'NONE',  ( 0.000000000000000000, 0.000000000000000000, 1.000000000000000000 ) ) ;
#3298 = CARTESIAN_POINT ( 'NONE',  ( 0.000000000000000000, 0.000000000000000000, 0.000000000000000000 ) ) ;
#3299 = CARTESIAN_POINT ( 'NONE',  ( 4.138106518798946531, 8.052838533163340529, 6.857782953271941950E-17 ) ) ;
#3300 = EDGE_CURVE ( 'NONE', #9888, #363, #186, .T. ) ;
#3301 = AXIS2_PLACEMENT_3D ( 'NONE', #10748, #2426, #2614 ) ;
#3302 = CARTESIAN_POINT ( 'NONE',  ( 3.000000000000000888, 21.76479567747252020, -7.432877647174977120 ) ) ;
#3303 = VERTEX_POINT ( 'NONE', #6261 ) ;
#3304 = CARTESIAN_POINT ( 'NONE',  ( 3.000000000000000888, -22.83456483164687256, -2.745295967526231173 ) ) ;
#3305 = ORIENTED_EDGE ( 'NONE', *, *, #7322, .T. ) ;
#3306 = CARTESIAN_POINT ( 'NONE',  ( -8.109405675831295568, 8.372220220303479010, 10.00000000000000000 ) ) ;
#3307 = CIRCLE ( 'NONE', #3513, 9.599999999999997868 ) ;
#3308 = AXIS2_PLACEMENT_3D ( 'NONE', #11195, #9919, #11755 ) ;
#3309 = ORIENTED_EDGE ( 'NONE', *, *, #2304, .F. ) ;
#3310 = ADVANCED_FACE ( 'NONE', ( #3393 ), #504, .T. ) ;
#3311 = CARTESIAN_POINT ( 'NONE',  ( 0.000000000000000000, 22.21333432029563681, 11.02759168516752908 ) ) ;
#3312 = CARTESIAN_POINT ( 'NONE',  ( 0.000000000000000000, -21.96011696265487600, -5.135568396240250522 ) ) ;
#3313 = VECTOR ( 'NONE', #7068, 1000.000000000000000 ) ;
#3314 = PLANE ( 'NONE',  #5235 ) ;
#3315 = DIRECTION ( 'NONE',  ( 0.000000000000000000, 0.000000000000000000, 1.000000000000000000 ) ) ;
#3316 = CARTESIAN_POINT ( 'NONE',  ( 1.018538006779725835, -7.771884277300785904, 10.00000000000000000 ) ) ;
#3317 = ADVANCED_FACE ( 'NONE', ( #10728 ), #4422, .T. ) ;
#3318 = AXIS2_PLACEMENT_3D ( 'NONE', #3773, #4687, #5790 ) ;
#3319 = CARTESIAN_POINT ( 'NONE',  ( 0.000000000000000000, -22.47229024614976112, -1.901833551798492561 ) ) ;
#3320 = CARTESIAN_POINT ( 'NONE',  ( -11.98301361336074145, 0.7816210414391653316, 3.747395293195558847E-16 ) ) ;
#3321 = CARTESIAN_POINT ( 'NONE',  ( 3.000000000000000888, 15.13242714128119459, 17.31945870441152380 ) ) ;
#3322 = ORIENTED_EDGE ( 'NONE', *, *, #1903, .T. ) ;
#3323 = CYLINDRICAL_SURFACE ( 'NONE', #6845, 22.99899999999999878 ) ;
#3324 = AXIS2_PLACEMENT_3D ( 'NONE', #11526, #8777, #2285 ) ;
#3325 = ORIENTED_EDGE ( 'NONE', *, *, #5385, .T. ) ;
#3326 = EDGE_CURVE ( 'NONE', #384, #900, #5867, .T. ) ;
#3327 = DIRECTION ( 'NONE',  ( 0.000000000000000000, 0.9135454576426019768, -0.4067366430757979878 ) ) ;
#3328 = EDGE_LOOP ( 'NONE', ( #5144, #5130, #11701, #8794 ) ) ;
#3329 = CARTESIAN_POINT ( 'NONE',  ( 3.000000000000000888, -14.74749645580022772, 17.06259499759939402 ) ) ;
#3330 = VECTOR ( 'NONE', #10473, 1000.000000000000000 ) ;
#3331 = DIRECTION ( 'NONE',  ( 0.000000000000000000, 0.000000000000000000, -1.000000000000000000 ) ) ;
#3332 = DIRECTION ( 'NONE',  ( 0.000000000000000000, 0.000000000000000000, 1.000000000000000000 ) ) ;
#3333 = LINE ( 'NONE', #6156, #1596 ) ;
#3334 = CARTESIAN_POINT ( 'NONE',  ( -7.159234172427924925, 10.34564589702410942, 6.857782953271941950E-17 ) ) ;
#3335 =( GEOMETRIC_REPRESENTATION_CONTEXT ( 3 ) GLOBAL_UNCERTAINTY_ASSIGNED_CONTEXT ( ( #10022 ) ) GLOBAL_UNIT_ASSIGNED_CONTEXT ( ( #1330, #10642, #7821 ) ) REPRESENTATION_CONTEXT ( 'NONE', 'WORKASPACE' ) );
#3336 = CARTESIAN_POINT ( 'NONE',  ( -3.500000000000000000, 4.286263797015736595E-16, -15.00000000000000000 ) ) ;
#3337 = FACE_OUTER_BOUND ( 'NONE', #6109, .T. ) ;
#3338 = ORIENTED_EDGE ( 'NONE', *, *, #5457, .T. ) ;
#3339 = EDGE_CURVE ( 'NONE', #3644, #8566, #2738, .T. ) ;
#3340 = AXIS2_PLACEMENT_3D ( 'NONE', #11217, #11939, #10048 ) ;
#3341 = ORIENTED_EDGE ( 'NONE', *, *, #682, .F. ) ;
#3342 = CIRCLE ( 'NONE', #11552, 24.80000000000000071 ) ;
#3343 = ORIENTED_EDGE ( 'NONE', *, *, #1341, .T. ) ;
#3344 = CARTESIAN_POINT ( 'NONE',  ( -7.594692469639083399, -9.901549393538205734, 10.00000000000000000 ) ) ;
#3345 = DIRECTION ( 'NONE',  ( -1.000000000000000000, 0.000000000000000000, 0.000000000000000000 ) ) ;
#3346 = DIRECTION ( 'NONE',  ( 0.000000000000000000, 0.000000000000000000, 1.000000000000000000 ) ) ;
#3347 = VECTOR ( 'NONE', #12014, 1000.000000000000000 ) ;
#3348 = AXIS2_PLACEMENT_3D ( 'NONE', #6351, #9101, #9154 ) ;
#3349 = AXIS2_PLACEMENT_3D ( 'NONE', #1377, #4138, #394 ) ;
#3350 = CARTESIAN_POINT ( 'NONE',  ( -8.834572391846261752, 1.442725564903823532, 3.747395293195558847E-16 ) ) ;
#3351 = CIRCLE ( 'NONE', #9608, 9.599999999999997868 ) ;
#3352 = CARTESIAN_POINT ( 'NONE',  ( 3.000000000000000888, -2.745295967525840375, -22.83456483164691875 ) ) ;
#3353 = LINE ( 'NONE', #1749, #7414 ) ;
#3354 = ORIENTED_EDGE ( 'NONE', *, *, #3195, .F. ) ;
#3355 = ORIENTED_EDGE ( 'NONE', *, *, #9344, .T. ) ;
#3356 = CONTEXT_DEPENDENT_SHAPE_REPRESENTATION ( #12000, #6672 ) ;
#3357 = CARTESIAN_POINT ( 'NONE',  ( -12.91830213043054698, -2.344901317288422327, 10.00000000000000000 ) ) ;
#3358 = AXIS2_PLACEMENT_3D ( 'NONE', #6198, #11821, #3387 ) ;
#3359 = EDGE_LOOP ( 'NONE', ( #4223, #7168, #1880, #7456 ) ) ;
#3360 = DIRECTION ( 'NONE',  ( 0.000000000000000000, 0.9510565162951544194, -0.3090169943749449533 ) ) ;
#3361 = CARTESIAN_POINT ( 'NONE',  ( 0.000000000000000000, 0.000000000000000000, 0.000000000000000000 ) ) ;
#3362 = DIRECTION ( 'NONE',  ( -2.303929616531696922E-17, 1.860490927985125609E-14, 1.000000000000000000 ) ) ;
#3363 = CIRCLE ( 'NONE', #11543, 22.99899999999999878 ) ;
#3364 = DIRECTION ( 'NONE',  ( 0.000000000000000000, 0.000000000000000000, 1.000000000000000000 ) ) ;
#3365 = VERTEX_POINT ( 'NONE', #6081 ) ;
#3366 = EDGE_CURVE ( 'NONE', #8825, #9990, #5282, .T. ) ;
#3367 = DIRECTION ( 'NONE',  ( 0.000000000000000000, 0.000000000000000000, 1.000000000000000000 ) ) ;
#3368 = ADVANCED_FACE ( 'NONE', ( #5350 ), #5162, .T. ) ;
#3369 = DIRECTION ( 'NONE',  ( -1.000000000000000000, -0.000000000000000000, -0.000000000000000000 ) ) ;
#3370 = CARTESIAN_POINT ( 'NONE',  ( 5.835571643920552276, -9.386589068694823013, 6.857782953271941950E-17 ) ) ;
#3371 = VECTOR ( 'NONE', #11665, 1000.000000000000000 ) ;
#3372 = AXIS2_PLACEMENT_3D ( 'NONE', #10706, #10523, #4168 ) ;
#3373 = DIRECTION ( 'NONE',  ( 0.000000000000000000, 0.000000000000000000, 1.000000000000000000 ) ) ;
#3374 = DIRECTION ( 'NONE',  ( 1.000000000000000000, -0.000000000000000000, -0.000000000000000000 ) ) ;
#3375 = ORIENTED_EDGE ( 'NONE', *, *, #455, .F. ) ;
#3376 = CARTESIAN_POINT ( 'NONE',  ( -11.62103867303406979, 2.700230667072889279, 10.00000000000000000 ) ) ;
#3377 = ADVANCED_FACE ( 'NONE', ( #7968 ), #1668, .T. ) ;
#3378 = VECTOR ( 'NONE', #8494, 1000.000000000000000 ) ;
#3379 = CARTESIAN_POINT ( 'NONE',  ( 3.000000000000000888, 6.168200451486087310, -24.02068490260606382 ) ) ;
#3380 = CARTESIAN_POINT ( 'NONE',  ( 3.000000000000000888, -9.128825345753185161, 23.05871956130119216 ) ) ;
#3381 = ORIENTED_EDGE ( 'NONE', *, *, #6288, .F. ) ;
#3382 = ADVANCED_FACE ( 'NONE', ( #4362 ), #9080, .T. ) ;
#3383 = LINE ( 'NONE', #11818, #8366 ) ;
#3384 = CIRCLE ( 'NONE', #8477, 24.80000000000000071 ) ;
#3385 = DIRECTION ( 'NONE',  ( 0.000000000000000000, 0.3090169943749480064, -0.9510565162951533091 ) ) ;
#3386 = CARTESIAN_POINT ( 'NONE',  ( -8.201440678128605555, 5.289679325232168772, 10.00000000000000000 ) ) ;
#3387 = DIRECTION ( 'NONE',  ( 0.000000000000000000, 0.000000000000000000, 1.000000000000000000 ) ) ;
#3388 = CARTESIAN_POINT ( 'NONE',  ( 4.163410377374355598, -12.26152398776834040, 3.747395293195558847E-16 ) ) ;
#3389 = DIRECTION ( 'NONE',  ( -1.000000000000000000, -0.000000000000000000, 0.000000000000000000 ) ) ;
#3390 = AXIS2_PLACEMENT_3D ( 'NONE', #9007, #623, #4471 ) ;
#3391 = ORIENTED_EDGE ( 'NONE', *, *, #4685, .F. ) ;
#3392 = ORIENTED_EDGE ( 'NONE', *, *, #10688, .F. ) ;
#3393 = FACE_OUTER_BOUND ( 'NONE', #6614, .T. ) ;
#3394 = ORIENTED_EDGE ( 'NONE', *, *, #7697, .T. ) ;
#3395 = AXIS2_PLACEMENT_3D ( 'NONE', #2437, #718, #11975 ) ;
#3396 = AXIS2_PLACEMENT_3D ( 'NONE', #2281, #320, #3142 ) ;
#3397 = DIRECTION ( 'NONE',  ( 1.000000000000000000, 0.000000000000000000, 0.000000000000000000 ) ) ;
#3398 = ADVANCED_FACE ( 'NONE', ( #11702 ), #3323, .T. ) ;
#3399 = CARTESIAN_POINT ( 'NONE',  ( 3.000000000000000888, -15.42759117534374447, -16.45023496161680754 ) ) ;
#3400 = FILL_AREA_STYLE ('',( #816 ) ) ;
#3401 = ORIENTED_EDGE ( 'NONE', *, *, #4065, .F. ) ;
#3402 = CIRCLE ( 'NONE', #9256, 24.80000000000000071 ) ;
#3403 = CARTESIAN_POINT ( 'NONE',  ( 3.000000000000000888, -1.556492618230808089, 24.75110766671651419 ) ) ;
#3404 = CARTESIAN_POINT ( 'NONE',  ( 0.000000000000000000, 2.745295967526300451, -22.83456483164686546 ) ) ;
#3405 = CARTESIAN_POINT ( 'NONE',  ( 3.534825977509327366, -7.171832907601992879, 10.00000000000000000 ) ) ;
#3406 = CARTESIAN_POINT ( 'NONE',  ( 6.986659217179107095, 9.748146710219840472, 6.857782953271941950E-17 ) ) ;
#3407 = PRESENTATION_STYLE_ASSIGNMENT (( #11779 ) ) ;
#3408 = CARTESIAN_POINT ( 'NONE',  ( 0.000000000000000000, -11.48910920600668462, -21.97817939804051690 ) ) ;
#3409 = ORIENTED_EDGE ( 'NONE', *, *, #9344, .F. ) ;
#3410 = AXIS2_PLACEMENT_3D ( 'NONE', #10493, #3952, #8668 ) ;
#3411 = ORIENTED_EDGE ( 'NONE', *, *, #11974, .F. ) ;
#3412 = AXIS2_PLACEMENT_3D ( 'NONE', #453, #512, #7974 ) ;
#3413 = ORIENTED_EDGE ( 'NONE', *, *, #5617, .F. ) ;
#3414 = EDGE_CURVE ( 'NONE', #7118, #4299, #11646, .T. ) ;
#3415 = CARTESIAN_POINT ( 'NONE',  ( -13.29946171776686903, 6.562258890817373569, 10.00000000000000000 ) ) ;
#3416 = SURFACE_STYLE_USAGE ( .BOTH. , #4320 ) ;
#3417 = CARTESIAN_POINT ( 'NONE',  ( 3.000000000000000888, 18.80635025205169697, 13.23915371906961447 ) ) ;
#3418 = CIRCLE ( 'NONE', #5766, 22.99899999999999878 ) ;
#3419 = EDGE_CURVE ( 'NONE', #3959, #10471, #9926, .T. ) ;
#3420 = CARTESIAN_POINT ( 'NONE',  ( 5.892341078160108658, -4.186101517074008349, 3.747395293195558847E-16 ) ) ;
#3421 = CARTESIAN_POINT ( 'NONE',  ( 3.000000000000000888, 0.3433949777334901476, -22.99643626497956461 ) ) ;
#3422 = DIRECTION ( 'NONE',  ( 0.000000000000000000, 0.000000000000000000, -1.000000000000000000 ) ) ;
#3423 = ORIENTED_EDGE ( 'NONE', *, *, #1149, .T. ) ;
#3424 = ORIENTED_EDGE ( 'NONE', *, *, #7207, .T. ) ;
#3425 = APPLICATION_PROTOCOL_DEFINITION ( 'draft international standard', 'automotive_design', 1998, #9271 ) ;
#3426 = ORIENTED_EDGE ( 'NONE', *, *, #361, .F. ) ;
#3427 = CARTESIAN_POINT ( 'NONE',  ( 0.3190826481552657135, -3.778307095988849618, 10.00000000000000000 ) ) ;
#3428 = AXIS2_PLACEMENT_3D ( 'NONE', #5580, #4838, #11147 ) ;
#3429 = DIRECTION ( 'NONE',  ( -1.000000000000000000, 0.000000000000000000, 0.000000000000000000 ) ) ;
#3430 = DIRECTION ( 'NONE',  ( 1.000000000000000000, 0.000000000000000000, -0.000000000000000000 ) ) ;
#3431 = CYLINDRICAL_SURFACE ( 'NONE', #4851, 24.80000000000000071 ) ;
#3432 = EDGE_LOOP ( 'NONE', ( #6111, #4906, #2197, #6743 ) ) ;
#3433 = CARTESIAN_POINT ( 'NONE',  ( 3.000000000000000888, -9.128825345752879628, -23.05871956130131650 ) ) ;
#3434 = DIRECTION ( 'NONE',  ( 0.000000000000000000, -0.8660254037844433705, 0.4999999999999919509 ) ) ;
#3435 = CARTESIAN_POINT ( 'NONE',  ( -6.589974825828272209, 7.038139701356662670, 6.857782953271941950E-17 ) ) ;
#3436 = CARTESIAN_POINT ( 'NONE',  ( 0.000000000000000000, 13.23915371906955052, 18.80635025205174671 ) ) ;
#3437 = DIRECTION ( 'NONE',  ( 0.000000000000000000, 0.000000000000000000, 1.000000000000000000 ) ) ;
#3438 = ORIENTED_EDGE ( 'NONE', *, *, #901, .T. ) ;
#3439 = CARTESIAN_POINT ( 'NONE',  ( -3.663109177303994546, -5.348850660921632638, 10.00000000000000000 ) ) ;
#3440 = ORIENTED_EDGE ( 'NONE', *, *, #9025, .T. ) ;
#3441 = DIRECTION ( 'NONE',  ( -1.000000000000000000, 0.000000000000000000, -0.000000000000000000 ) ) ;
#3442 = EDGE_CURVE ( 'NONE', #4464, #4944, #5290, .T. ) ;
#3443 = CARTESIAN_POINT ( 'NONE',  ( 1.499999999999999556, 24.45282072769601101, 4.135161237383664812 ) ) ;
#3444 = CARTESIAN_POINT ( 'NONE',  ( 0.000000000000000000, 0.000000000000000000, 0.000000000000000000 ) ) ;
#3445 = CARTESIAN_POINT ( 'NONE',  ( -1.916691774771272172, -10.52688368019216725, 10.00000000000000000 ) ) ;
#3446 = DIRECTION ( 'NONE',  ( -1.000000000000000000, 0.000000000000000000, 0.000000000000000000 ) ) ;
#3447 = CARTESIAN_POINT ( 'NONE',  ( -2.069312577552832266, -12.54440658741723880, 3.747395293195558847E-16 ) ) ;
#3448 = EDGE_CURVE ( 'NONE', #994, #6849, #11727, .T. ) ;
#3449 = CARTESIAN_POINT ( 'NONE',  ( 3.000000000000000888, -18.40266524480579236, -13.79477846460815194 ) ) ;
#3450 = VERTEX_POINT ( 'NONE', #3453 ) ;
#3451 = VECTOR ( 'NONE', #11224, 1000.000000000000000 ) ;
#3452 = ORIENTED_EDGE ( 'NONE', *, *, #3256, .F. ) ;
#3453 = CARTESIAN_POINT ( 'NONE',  ( 16.50000000000000000, 0.000000000000000000, 3.747395293195558847E-16 ) ) ;
#3454 = EDGE_CURVE ( 'NONE', #1309, #215, #3, .T. ) ;
#3455 = VERTEX_POINT ( 'NONE', #7223 ) ;
#3456 = EDGE_CURVE ( 'NONE', #10077, #4242, #8427, .T. ) ;
#3457 = CARTESIAN_POINT ( 'NONE',  ( 0.9209971296404340091, -6.773236541304579639, 3.747395293195558847E-16 ) ) ;
#3458 = DIRECTION ( 'NONE',  ( 1.000000000000000000, -0.000000000000000000, 0.000000000000000000 ) ) ;
#3459 =( NAMED_UNIT ( * ) SI_UNIT ( $, .STERADIAN. ) SOLID_ANGLE_UNIT ( ) );
#3460 = VERTEX_POINT ( 'NONE', #10051 ) ;
#3461 = FACE_OUTER_BOUND ( 'NONE', #9345, .T. ) ;
#3462 = CIRCLE ( 'NONE', #2272, 24.80000000000000071 ) ;
#3463 = DIRECTION ( 'NONE',  ( 0.000000000000000000, -0.9781476007338034684, -0.2079116908177697509 ) ) ;
#3464 = CARTESIAN_POINT ( 'NONE',  ( 0.000000000000000000, 20.93895013827599882, -13.28910708463105728 ) ) ;
#3465 = CARTESIAN_POINT ( 'NONE',  ( -3.764233030011072678, -6.516208816467838894, 10.00000000000000000 ) ) ;
#3466 = CARTESIAN_POINT ( 'NONE',  ( 3.343943643650757913, -10.41127694127634129, 6.857782953271941950E-17 ) ) ;
#3467 = CARTESIAN_POINT ( 'NONE',  ( 0.000000000000000000, -1.901833551798412847, 22.47229024614976822 ) ) ;
#3468 = DIRECTION ( 'NONE',  ( -1.000000000000000000, 0.000000000000000000, 0.000000000000000000 ) ) ;
#3469 = VERTEX_POINT ( 'NONE', #2836 ) ;
#3470 = ORIENTED_EDGE ( 'NONE', *, *, #2771, .T. ) ;
#3471 = ORIENTED_EDGE ( 'NONE', *, *, #3300, .F. ) ;
#3472 = CARTESIAN_POINT ( 'NONE',  ( -11.98301361336074500, 0.7816210414391656647, 10.00000000000000000 ) ) ;
#3473 = DIRECTION ( 'NONE',  ( -1.000000000000000000, 0.000000000000000000, 0.000000000000000000 ) ) ;
#3474 = EDGE_CURVE ( 'NONE', #7835, #9404, #9258, .T. ) ;
#3475 = DIRECTION ( 'NONE',  ( 1.000000000000000000, 0.000000000000000000, 0.000000000000000000 ) ) ;
#3476 = CARTESIAN_POINT ( 'NONE',  ( -3.038216613429991053, 4.635879136410029133, 3.747395293195558847E-16 ) ) ;
#3477 = ADVANCED_FACE ( 'NONE', ( #11220 ), #10350, .T. ) ;
#3478 = AXIS2_PLACEMENT_3D ( 'NONE', #9264, #11888, #11774 ) ;
#3479 = DIRECTION ( 'NONE',  ( 1.000000000000000000, -0.000000000000000000, 0.000000000000000000 ) ) ;
#3480 = DIRECTION ( 'NONE',  ( 1.000000000000000000, 0.000000000000000000, 0.000000000000000000 ) ) ;
#3481 = ORIENTED_EDGE ( 'NONE', *, *, #510, .T. ) ;
#3482 = EDGE_LOOP ( 'NONE', ( #7823, #9576, #6820, #10091 ) ) ;
#3483 = EDGE_CURVE ( 'NONE', #10348, #11545, #5096, .T. ) ;
#3484 = ORIENTED_EDGE ( 'NONE', *, *, #1488, .T. ) ;
#3485 = CARTESIAN_POINT ( 'NONE',  ( 4.516389116325776776, 1.247036727255508737, 10.00000000000000000 ) ) ;
#3486 = FACE_OUTER_BOUND ( 'NONE', #4348, .T. ) ;
#3487 = EDGE_CURVE ( 'NONE', #992, #6788, #7409, .T. ) ;
#3488 = CYLINDRICAL_SURFACE ( 'NONE', #3494, 24.80000000000000071 ) ;
#3489 = ORIENTED_EDGE ( 'NONE', *, *, #669, .T. ) ;
#3490 = CARTESIAN_POINT ( 'NONE',  ( -10.00000000000000000, 0.000000000000000000, 0.000000000000000000 ) ) ;
#3491 = DIRECTION ( 'NONE',  ( -1.000000000000000000, -0.000000000000000000, -0.000000000000000000 ) ) ;
#3492 = CARTESIAN_POINT ( 'NONE',  ( -5.152979166089614260, -5.321787192520350374, 6.857782953271941950E-17 ) ) ;
#3493 = DIRECTION ( 'NONE',  ( 1.000000000000000000, 0.000000000000000000, 0.000000000000000000 ) ) ;
#3494 = AXIS2_PLACEMENT_3D ( 'NONE', #7197, #2565, #1647 ) ;
#3495 = DIRECTION ( 'NONE',  ( 0.000000000000000000, 0.000000000000000000, 1.000000000000000000 ) ) ;
#3496 = VERTEX_POINT ( 'NONE', #2648 ) ;
#3497 = ORIENTED_EDGE ( 'NONE', *, *, #9146, .F. ) ;
#3498 = CARTESIAN_POINT ( 'NONE',  ( -0.4771094043438766641, 5.286185534804332065, 10.00000000000000000 ) ) ;
#3499 = ORIENTED_EDGE ( 'NONE', *, *, #4122, .T. ) ;
#3500 = FACE_OUTER_BOUND ( 'NONE', #9093, .T. ) ;
#3501 = ORIENTED_EDGE ( 'NONE', *, *, #4499, .F. ) ;
#3502 = CIRCLE ( 'NONE', #10332, 22.99899999999999878 ) ;
#3503 = DIRECTION ( 'NONE',  ( -1.000000000000000000, -0.000000000000000000, 0.000000000000000000 ) ) ;
#3504 = AXIS2_PLACEMENT_3D ( 'NONE', #10801, #5533, #1794 ) ;
#3505 = CARTESIAN_POINT ( 'NONE',  ( -10.00000000000000000, 0.000000000000000000, 0.000000000000000000 ) ) ;
#3506 = CARTESIAN_POINT ( 'NONE',  ( -0.1504880127287666625, 9.287785325659767111, 10.00000000000000000 ) ) ;
#3507 = DIRECTION ( 'NONE',  ( 0.000000000000000000, 0.000000000000000000, 1.000000000000000000 ) ) ;
#3508 = CARTESIAN_POINT ( 'NONE',  ( 3.000000000000000888, 17.35216073792440739, 17.71842311621536226 ) ) ;
#3509 = VERTEX_POINT ( 'NONE', #3572 ) ;
#3510 = ORIENTED_EDGE ( 'NONE', *, *, #6940, .T. ) ;
#3511 = DIRECTION ( 'NONE',  ( 0.000000000000000000, -0.1045284632676605485, 0.9945218953682725127 ) ) ;
#3512 = EDGE_LOOP ( 'NONE', ( #11119, #3426 ) ) ;
#3513 = AXIS2_PLACEMENT_3D ( 'NONE', #2561, #1645, #9109 ) ;
#3514 = CARTESIAN_POINT ( 'NONE',  ( 4.516389116325773223, 1.247036727255508515, 3.747395293195558847E-16 ) ) ;
#3515 = LINE ( 'NONE', #6332, #6560 ) ;
#3516 = VERTEX_POINT ( 'NONE', #1970 ) ;
#3517 = CARTESIAN_POINT ( 'NONE',  ( 0.000000000000000000, 0.000000000000000000, 0.000000000000000000 ) ) ;
#3518 = EDGE_CURVE ( 'NONE', #7676, #11174, #9589, .T. ) ;
#3519 = DIRECTION ( 'NONE',  ( -0.000000000000000000, -0.000000000000000000, 1.000000000000000000 ) ) ;
#3520 = CARTESIAN_POINT ( 'NONE',  ( 5.267519402444160725, 2.381954139586888175, 10.00000000000000000 ) ) ;
#3521 = CARTESIAN_POINT ( 'NONE',  ( -9.352287007201468327, 3.176141031410556703, 6.857782953271941950E-17 ) ) ;
#3522 = DIRECTION ( 'NONE',  ( 0.000000000000000000, 0.9135454576425990902, 0.4067366430758041496 ) ) ;
#3523 = EDGE_CURVE ( 'NONE', #9646, #6735, #5456, .T. ) ;
#3524 = CARTESIAN_POINT ( 'NONE',  ( 3.000000000000000888, 4.240409074144097623, 22.15038895030650679 ) ) ;
#3525 = ORIENTED_EDGE ( 'NONE', *, *, #330, .T. ) ;
#3526 = ORIENTED_EDGE ( 'NONE', *, *, #11141, .F. ) ;
#3527 = CIRCLE ( 'NONE', #10978, 9.599999999999997868 ) ;
#3528 = CARTESIAN_POINT ( 'NONE',  ( 13.54728169684850414, 0.8932250400876640128, 10.00000000000000000 ) ) ;
#3529 = CIRCLE ( 'NONE', #10160, 9.599999999999997868 ) ;
#3530 = EDGE_CURVE ( 'NONE', #3286, #4143, #7830, .T. ) ;
#3531 = DIRECTION ( 'NONE',  ( -1.000000000000000000, -0.000000000000000000, 0.000000000000000000 ) ) ;
#3532 = CARTESIAN_POINT ( 'NONE',  ( 3.000000000000000888, 0.000000000000000000, 0.000000000000000000 ) ) ;
#3533 = CARTESIAN_POINT ( 'NONE',  ( -1.515734900794040385, 8.225284064336934264, 3.747395293195558847E-16 ) ) ;
#3534 = VECTOR ( 'NONE', #4858, 1000.000000000000000 ) ;
#3535 = CARTESIAN_POINT ( 'NONE',  ( 3.000000000000000000, 0.000000000000000000, 0.000000000000000000 ) ) ;
#3536 = ORIENTED_EDGE ( 'NONE', *, *, #10780, .F. ) ;
#3537 = AXIS2_PLACEMENT_3D ( 'NONE', #4530, #11019, #2748 ) ;
#3538 = CYLINDRICAL_SURFACE ( 'NONE', #1960, 24.80000000000000071 ) ;
#3539 = EDGE_LOOP ( 'NONE', ( #356, #6886, #7903, #1472 ) ) ;
#3540 = EDGE_CURVE ( 'NONE', #8199, #8745, #1762, .T. ) ;
#3541 = VERTEX_POINT ( 'NONE', #6382 ) ;
#3542 = CARTESIAN_POINT ( 'NONE',  ( 3.000000000000000888, 0.000000000000000000, 0.000000000000000000 ) ) ;
#3543 = CARTESIAN_POINT ( 'NONE',  ( 0.000000000000000000, 0.000000000000000000, 4.000000000000000000 ) ) ;
#3544 = EDGE_CURVE ( 'NONE', #10492, #1145, #10372, .T. ) ;
#3545 = AXIS2_PLACEMENT_3D ( 'NONE', #7651, #3014, #6734 ) ;
#3546 = DIRECTION ( 'NONE',  ( -0.000000000000000000, -0.000000000000000000, 1.000000000000000000 ) ) ;
#3547 = CIRCLE ( 'NONE', #6281, 19.99999999999999645 ) ;
#3548 = DIRECTION ( 'NONE',  ( 0.000000000000000000, 0.000000000000000000, -1.000000000000000000 ) ) ;
#3549 = DIRECTION ( 'NONE',  ( 0.000000000000000000, 0.000000000000000000, 1.000000000000000000 ) ) ;
#3550 = CARTESIAN_POINT ( 'NONE',  ( 2.004495162477540671, 5.838205294495789843, 6.857782953271941950E-17 ) ) ;
#3551 = LINE ( 'NONE', #9299, #793 ) ;
#3552 = ORIENTED_EDGE ( 'NONE', *, *, #1649, .F. ) ;
#3553 = CIRCLE ( 'NONE', #387, 9.599999999999996092 ) ;
#3554 = DIRECTION ( 'NONE',  ( -1.000000000000000000, -0.000000000000000000, 0.000000000000000000 ) ) ;
#3555 = VECTOR ( 'NONE', #4435, 1000.000000000000000 ) ;
#3556 = VERTEX_POINT ( 'NONE', #7284 ) ;
#3557 = ORIENTED_EDGE ( 'NONE', *, *, #2263, .F. ) ;
#3558 = CARTESIAN_POINT ( 'NONE',  ( -0.7379871813790722657, -6.677365878963855472, 10.00000000000000000 ) ) ;
#3559 = EDGE_CURVE ( 'NONE', #5600, #9959, #7619, .T. ) ;
#3560 = VERTEX_POINT ( 'NONE', #1911 ) ;
#3561 = CARTESIAN_POINT ( 'NONE',  ( 3.000000000000000888, 6.532525787310969001, 21.58580335785678983 ) ) ;
#3562 = VERTEX_POINT ( 'NONE', #7346 ) ;
#3563 = MECHANICAL_DESIGN_GEOMETRIC_PRESENTATION_REPRESENTATION (  '', ( #7661 ), #8844 ) ;
#3564 = CIRCLE ( 'NONE', #2386, 1.500000000000000222 ) ;
#3565 = DIRECTION ( 'NONE',  ( 0.000000000000000000, 0.000000000000000000, 1.000000000000000000 ) ) ;
#3566 = DIRECTION ( 'NONE',  ( -1.000000000000000000, 0.000000000000000000, -0.000000000000000000 ) ) ;
#3567 = CARTESIAN_POINT ( 'NONE',  ( 17.49999999999999645, 0.000000000000000000, 6.857782953271941950E-17 ) ) ;
#3568 = DIRECTION ( 'NONE',  ( 0.000000000000000000, 0.9945218953682737340, -0.1045284632676502651 ) ) ;
#3569 = EDGE_CURVE ( 'NONE', #7896, #11364, #11090, .T. ) ;
#3570 = CARTESIAN_POINT ( 'NONE',  ( 3.000000000000000888, -22.56530478845651544, 4.445336973060782348 ) ) ;
#3571 = ORIENTED_EDGE ( 'NONE', *, *, #7802, .F. ) ;
#3572 = CARTESIAN_POINT ( 'NONE',  ( 0.000000000000000000, -15.40502424595132247, -19.43515443678418819 ) ) ;
#3573 = ORIENTED_EDGE ( 'NONE', *, *, #1964, .F. ) ;
#3574 = PRESENTATION_LAYER_ASSIGNMENT (  '', '', ( #8851 ) ) ;
#3575 = CARTESIAN_POINT ( 'NONE',  ( 0.3190826481552654914, -3.778307095988950870, 3.747395293195558847E-16 ) ) ;
#3576 = AXIS2_PLACEMENT_3D ( 'NONE', #6768, #7690, #7810 ) ;
#3577 = DIRECTION ( 'NONE',  ( 0.000000000000000000, 0.000000000000000000, 1.000000000000000000 ) ) ;
#3578 = DIRECTION ( 'NONE',  ( 0.000000000000000000, 0.000000000000000000, 1.000000000000000000 ) ) ;
#3579 = CARTESIAN_POINT ( 'NONE',  ( 3.000000000000000888, -13.62355943574006645, -17.97274125076088680 ) ) ;
#3580 = CARTESIAN_POINT ( 'NONE',  ( -5.101271054653082615, -15.85638610327791476, 10.00000000000000000 ) ) ;
#3581 = AXIS2_PLACEMENT_3D ( 'NONE', #11872, #3503, #2642 ) ;
#3582 = CARTESIAN_POINT ( 'NONE',  ( -2.682496113117365244, -7.114254743909630641, 6.857782953271941950E-17 ) ) ;
#3583 = CARTESIAN_POINT ( 'NONE',  ( 0.000000000000000000, 19.74380051311539930, 11.79560690673879186 ) ) ;
#3584 = DIRECTION ( 'NONE',  ( -1.000000000000000000, 0.000000000000000000, -0.000000000000000000 ) ) ;
#3585 = AXIS2_PLACEMENT_3D ( 'NONE', #11853, #10942, #535 ) ;
#3586 = CIRCLE ( 'NONE', #7276, 9.599999999999996092 ) ;
#3587 = ORIENTED_EDGE ( 'NONE', *, *, #8008, .F. ) ;
#3588 = ORIENTED_EDGE ( 'NONE', *, *, #3569, .T. ) ;
#3589 = VECTOR ( 'NONE', #11859, 1000.000000000000000 ) ;
#3590 = CARTESIAN_POINT ( 'NONE',  ( -12.61273389267918610, -8.731886703670456384, 10.00000000000000000 ) ) ;
#3591 = ADVANCED_FACE ( 'NONE', ( #6501 ), #6439, .T. ) ;
#3592 = CARTESIAN_POINT ( 'NONE',  ( 3.000000000000000888, 0.000000000000000000, 0.000000000000000000 ) ) ;
#3593 = CARTESIAN_POINT ( 'NONE',  ( -10.00000000000000000, 0.000000000000000000, 0.000000000000000000 ) ) ;
#3594 = EDGE_CURVE ( 'NONE', #2892, #1098, #4670, .T. ) ;
#3595 = CARTESIAN_POINT ( 'NONE',  ( 3.678979105947487671, -2.215585777442455662, 3.747395293195558847E-16 ) ) ;
#3596 = DIRECTION ( 'NONE',  ( 0.000000000000000000, 0.000000000000000000, -1.000000000000000000 ) ) ;
#3597 = ORIENTED_EDGE ( 'NONE', *, *, #2012, .F. ) ;
#3598 = EDGE_CURVE ( 'NONE', #1833, #9333, #9002, .T. ) ;
#3599 = DIRECTION ( 'NONE',  ( 0.000000000000000000, 0.000000000000000000, 1.000000000000000000 ) ) ;
#3600 = VERTEX_POINT ( 'NONE', #2 ) ;
#3601 = ORIENTED_EDGE ( 'NONE', *, *, #72, .T. ) ;
#3602 = ADVANCED_FACE ( 'NONE', ( #3752 ), #5645, .T. ) ;
#3603 = ORIENTED_EDGE ( 'NONE', *, *, #8034, .F. ) ;
#3604 = CARTESIAN_POINT ( 'NONE',  ( 4.340769014460005515, -0.9713985772308084687, 10.00000000000000000 ) ) ;
#3605 = EDGE_CURVE ( 'NONE', #5315, #4337, #2894, .T. ) ;
#3606 = DIRECTION ( 'NONE',  ( -1.000000000000000000, 0.000000000000000000, 0.000000000000000000 ) ) ;
#3607 = CIRCLE ( 'NONE', #275, 22.99899999999999878 ) ;
#3608 = CARTESIAN_POINT ( 'NONE',  ( 3.000000000000000888, -0.3433949777330061459, -22.99643626497957172 ) ) ;
#3609 = CARTESIAN_POINT ( 'NONE',  ( 3.000000000000000888, -23.24434456306330787, 8.645255683528924706 ) ) ;
#3610 = FACE_OUTER_BOUND ( 'NONE', #11502, .T. ) ;
#3611 = DIRECTION ( 'NONE',  ( -1.000000000000000000, 0.000000000000000000, 0.000000000000000000 ) ) ;
#3612 = DIRECTION ( 'NONE',  ( -1.000000000000000000, -0.000000000000000000, 0.000000000000000000 ) ) ;
#3613 = DIRECTION ( 'NONE',  ( 0.000000000000000000, 0.1045284632676538872, -0.9945218953682732899 ) ) ;
#3614 = AXIS2_PLACEMENT_3D ( 'NONE', #3505, #1717, #5451 ) ;
#3615 = ORIENTED_EDGE ( 'NONE', *, *, #5180, .F. ) ;
#3616 = CARTESIAN_POINT ( 'NONE',  ( 3.000000000000000888, -11.67026512804534022, -19.29833442572371638 ) ) ;
#3617 = ORIENTED_EDGE ( 'NONE', *, *, #5534, .T. ) ;
#3618 = CARTESIAN_POINT ( 'NONE',  ( 7.357672848543034050, 2.125097602832379806, 10.00000000000000000 ) ) ;
#3619 = ORIENTED_EDGE ( 'NONE', *, *, #10045, .F. ) ;
#3620 = CARTESIAN_POINT ( 'NONE',  ( 1.499999999999999556, 20.93895013827599882, -13.28910708463105905 ) ) ;
#3621 = ORIENTED_EDGE ( 'NONE', *, *, #11008, .F. ) ;
#3622 = FACE_OUTER_BOUND ( 'NONE', #7926, .T. ) ;
#3623 = DIRECTION ( 'NONE',  ( -1.000000000000000000, -0.000000000000000000, 0.000000000000000000 ) ) ;
#3624 = CARTESIAN_POINT ( 'NONE',  ( -15.56595607421883365, -4.438723023272252100, 6.857782953271941950E-17 ) ) ;
#3625 = DIRECTION ( 'NONE',  ( -1.000000000000000000, 0.000000000000000000, -0.000000000000000000 ) ) ;
#3626 = ADVANCED_FACE ( 'NONE', ( #11941 ), #2211, .T. ) ;
#3627 = DIRECTION ( 'NONE',  ( 0.000000000000000000, 0.000000000000000000, 1.000000000000000000 ) ) ;
#3628 = ORIENTED_EDGE ( 'NONE', *, *, #2645, .F. ) ;
#3629 = DIRECTION ( 'NONE',  ( -1.000000000000000000, -0.000000000000000000, 0.000000000000000000 ) ) ;
#3630 = VERTEX_POINT ( 'NONE', #9621 ) ;
#3631 = AXIS2_PLACEMENT_3D ( 'NONE', #10369, #1992, #3886 ) ;
#3632 = CARTESIAN_POINT ( 'NONE',  ( -5.069009347565034851, 2.772702716244574095, 3.747395293195558847E-16 ) ) ;
#3633 = DIRECTION ( 'NONE',  ( -1.000000000000000000, -0.000000000000000000, 0.000000000000000000 ) ) ;
#3634 =( LENGTH_UNIT ( ) NAMED_UNIT ( * ) SI_UNIT ( .MILLI., .METRE. ) );
#3635 = ADVANCED_FACE ( 'NONE', ( #8586 ), #7720, .T. ) ;
#3636 = CYLINDRICAL_SURFACE ( 'NONE', #1317, 24.80000000000000071 ) ;
#3637 = CARTESIAN_POINT ( 'NONE',  ( 0.000000000000000000, 18.51065745848395849, -12.88318129270159673 ) ) ;
#3638 = CARTESIAN_POINT ( 'NONE',  ( 3.000000000000000888, -22.15038895030646060, -4.240409074144325885 ) ) ;
#3639 = CARTESIAN_POINT ( 'NONE',  ( 15.92723891616543774, -6.911623607273383207, 10.00000000000000000 ) ) ;
#3640 = CIRCLE ( 'NONE', #4220, 24.80000000000000071 ) ;
#3641 = CARTESIAN_POINT ( 'NONE',  ( 2.004495162477540671, 5.838205294495789843, 6.857782953271941950E-17 ) ) ;
#3642 = DIRECTION ( 'NONE',  ( -1.000000000000000000, -0.000000000000000000, 0.000000000000000000 ) ) ;
#3643 = CARTESIAN_POINT ( 'NONE',  ( 0.000000000000000000, 0.000000000000000000, 0.000000000000000000 ) ) ;
#3644 = VERTEX_POINT ( 'NONE', #4909 ) ;
#3645 = ORIENTED_EDGE ( 'NONE', *, *, #10819, .T. ) ;
#3646 = VECTOR ( 'NONE', #2316, 1000.000000000000000 ) ;
#3647 = DIRECTION ( 'NONE',  ( 0.000000000000000000, 0.7431448254773954654, -0.6691306063588569053 ) ) ;
#3648 = CARTESIAN_POINT ( 'NONE',  ( 8.429646098664189680, -5.822225404888640377, 10.00000000000000000 ) ) ;
#3649 = CARTESIAN_POINT ( 'NONE',  ( 0.000000000000000000, -0.3433949777330061459, -22.99643626497957172 ) ) ;
#3650 = CYLINDRICAL_SURFACE ( 'NONE', #9938, 3.500000000000000000 ) ;
#3651 = CARTESIAN_POINT ( 'NONE',  ( -8.694522232909450921, -2.966707450564700199, 3.747395293195558847E-16 ) ) ;
#3652 = CARTESIAN_POINT ( 'NONE',  ( 4.525508228541170297, -0.2388087992699348128, 3.747395293195558847E-16 ) ) ;
#3653 = DIRECTION ( 'NONE',  ( 0.000000000000000000, -0.4067366430758070917, 0.9135454576425978690 ) ) ;
#3654 = EDGE_LOOP ( 'NONE', ( #1516, #11152, #7871, #2286 ) ) ;
#3655 = ORIENTED_EDGE ( 'NONE', *, *, #8462, .T. ) ;
#3656 = DIRECTION ( 'NONE',  ( 1.000000000000000000, 0.000000000000000000, 0.000000000000000000 ) ) ;
#3657 = EDGE_CURVE ( 'NONE', #3187, #1049, #1171, .T. ) ;
#3658 = DIRECTION ( 'NONE',  ( 0.000000000000000000, -0.8660254037844432595, 0.4999999999999919509 ) ) ;
#3659 = DIRECTION ( 'NONE',  ( 0.000000000000000000, -0.4999999999999887867, -0.8660254037844452579 ) ) ;
#3660 = CARTESIAN_POINT ( 'NONE',  ( 0.000000000000000000, 22.37663021667340146, 2.811977935938166695 ) ) ;
#3661 = CYLINDRICAL_SURFACE ( 'NONE', #6520, 22.99899999999999878 ) ;
#3662 = EDGE_CURVE ( 'NONE', #9763, #8613, #9978, .T. ) ;
#3663 = CARTESIAN_POINT ( 'NONE',  ( 12.25096627321951814, 6.291700371256212065, 3.747395293195558847E-16 ) ) ;
#3664 = CARTESIAN_POINT ( 'NONE',  ( -0.2556890074706221205, -7.756263830888991961, 6.857782953271941950E-17 ) ) ;
#3665 = EDGE_CURVE ( 'NONE', #4817, #10068, #1236, .T. ) ;
#3666 = DIRECTION ( 'NONE',  ( -1.000000000000000000, 0.000000000000000000, -0.000000000000000000 ) ) ;
#3667 = ORIENTED_EDGE ( 'NONE', *, *, #4870, .T. ) ;
#3668 = ORIENTED_EDGE ( 'NONE', *, *, #4723, .F. ) ;
#3669 = DIRECTION ( 'NONE',  ( 0.000000000000000000, -0.8090169943749526693, 0.5877852522924660317 ) ) ;
#3670 = ORIENTED_EDGE ( 'NONE', *, *, #4237, .F. ) ;
#3671 = AXIS2_PLACEMENT_3D ( 'NONE', #5152, #6800, #2219 ) ;
#3672 = ORIENTED_EDGE ( 'NONE', *, *, #1574, .F. ) ;
#3673 = CARTESIAN_POINT ( 'NONE',  ( -5.541928854458318732, -2.884958602215172974, 10.00000000000000000 ) ) ;
#3674 = ORIENTED_EDGE ( 'NONE', *, *, #2220, .F. ) ;
#3675 = CARTESIAN_POINT ( 'NONE',  ( 3.000000000000000888, -15.64281154287608722, 16.85990652506894705 ) ) ;
#3676 = ORIENTED_EDGE ( 'NONE', *, *, #1800, .T. ) ;
#3677 = EDGE_CURVE ( 'NONE', #2252, #9316, #3920, .T. ) ;
#3678 = DIRECTION ( 'NONE',  ( -1.000000000000000000, 0.000000000000000000, 0.000000000000000000 ) ) ;
#3679 = FACE_OUTER_BOUND ( 'NONE', #7043, .T. ) ;
#3680 = CARTESIAN_POINT ( 'NONE',  ( -6.451445390047177320, -3.308750875808899483, 10.00000000000000000 ) ) ;
#3681 = AXIS2_PLACEMENT_3D ( 'NONE', #1521, #8131, #10831 ) ;
#3682 = AXIS2_PLACEMENT_3D ( 'NONE', #9836, #1386, #3279 ) ;
#3683 = CARTESIAN_POINT ( 'NONE',  ( 0.000000000000000000, -19.43515443678392529, -15.40502424595165110 ) ) ;
#3684 = DIRECTION ( 'NONE',  ( -1.000000000000000000, -0.000000000000000000, -0.000000000000000000 ) ) ;
#3685 = ORIENTED_EDGE ( 'NONE', *, *, #10130, .T. ) ;
#3686 = ORIENTED_EDGE ( 'NONE', *, *, #6441, .T. ) ;
#3687 = DIRECTION ( 'NONE',  ( 0.000000000000000000, 0.9945218953682737340, -0.1045284632676502373 ) ) ;
#3688 = EDGE_LOOP ( 'NONE', ( #8294, #3501, #10227, #5318 ) ) ;
#3689 = EDGE_CURVE ( 'NONE', #5192, #10351, #11155, .T. ) ;
#3690 = CARTESIAN_POINT ( 'NONE',  ( 7.195390336726608105, 2.736402267197653337, 3.747395293195558847E-16 ) ) ;
#3691 = AXIS2_PLACEMENT_3D ( 'NONE', #5134, #10646, #10518 ) ;
#3692 = AXIS2_PLACEMENT_3D ( 'NONE', #6399, #5550, #3710 ) ;
#3693 = CARTESIAN_POINT ( 'NONE',  ( 3.000000000000000888, 8.645255683529311952, -23.24434456306316577 ) ) ;
#3694 = EDGE_CURVE ( 'NONE', #1936, #3509, #1292, .T. ) ;
#3695 = DIRECTION ( 'NONE',  ( 0.000000000000000000, 0.000000000000000000, -1.000000000000000000 ) ) ;
#3696 = CYLINDRICAL_SURFACE ( 'NONE', #9852, 20.00000000000000000 ) ;
#3697 = CARTESIAN_POINT ( 'NONE',  ( 10.64229886435067840, -13.41933351754447834, 10.00000000000000000 ) ) ;
#3698 = LINE ( 'NONE', #132, #2763 ) ;
#3699 = DIRECTION ( 'NONE',  ( -1.000000000000000000, 0.000000000000000000, 0.000000000000000000 ) ) ;
#3700 = CIRCLE ( 'NONE', #9948, 9.599999999999996092 ) ;
#3701 = CARTESIAN_POINT ( 'NONE',  ( 0.000000000000000000, 0.000000000000000000, 0.000000000000000000 ) ) ;
#3702 = ORIENTED_EDGE ( 'NONE', *, *, #6580, .F. ) ;
#3703 = EDGE_CURVE ( 'NONE', #7676, #2929, #3994, .T. ) ;
#3704 = ORIENTED_EDGE ( 'NONE', *, *, #9712, .F. ) ;
#3705 = FACE_OUTER_BOUND ( 'NONE', #9244, .T. ) ;
#3706 = CARTESIAN_POINT ( 'NONE',  ( -8.984113827416489784, -1.502549133976348816, 10.00000000000000000 ) ) ;
#3707 = VECTOR ( 'NONE', #6302, 1000.000000000000000 ) ;
#3708 = CIRCLE ( 'NONE', #4689, 24.80000000000000071 ) ;
#3709 = DIRECTION ( 'NONE',  ( -1.000000000000000000, 0.000000000000000000, 0.000000000000000000 ) ) ;
#3710 = DIRECTION ( 'NONE',  ( 1.000000000000000000, 0.000000000000000000, -0.000000000000000000 ) ) ;
#3711 = DIRECTION ( 'NONE',  ( 0.000000000000000000, -6.982962677686266711E-15, 1.000000000000000000 ) ) ;
#3712 = CIRCLE ( 'NONE', #8407, 9.599999999999996092 ) ;
#3713 = CARTESIAN_POINT ( 'NONE',  ( -6.597323627731391582, 9.514359934151556786, 3.747395293195558847E-16 ) ) ;
#3714 = CARTESIAN_POINT ( 'NONE',  ( 3.000000000000000888, -20.93895013827572171, -13.28910708463150492 ) ) ;
#3715 = FACE_BOUND ( 'NONE', #2862, .T. ) ;
#3716 = ORIENTED_EDGE ( 'NONE', *, *, #5841, .F. ) ;
#3717 = AXIS2_PLACEMENT_3D ( 'NONE', #11765, #2342, #3511 ) ;
#3718 = VERTEX_POINT ( 'NONE', #8708 ) ;
#3719 = DIRECTION ( 'NONE',  ( -1.000000000000000000, 0.000000000000000000, 0.000000000000000000 ) ) ;
#3720 = CARTESIAN_POINT ( 'NONE',  ( 1.500000000000000444, -24.45282072769603587, 4.135161237383498722 ) ) ;
#3721 =( LENGTH_UNIT ( ) NAMED_UNIT ( * ) SI_UNIT ( .MILLI., .METRE. ) );
#3722 = LINE ( 'NONE', #6536, #545 ) ;
#3723 = AXIS2_PLACEMENT_3D ( 'NONE', #1183, #9509, #11467 ) ;
#3724 = CARTESIAN_POINT ( 'NONE',  ( 19.99999999999999645, 2.449293598294706119E-15, 0.000000000000000000 ) ) ;
#3725 = VECTOR ( 'NONE', #3815, 1000.000000000000000 ) ;
#3726 = CARTESIAN_POINT ( 'NONE',  ( -14.24631147015001886, -5.364320868109360596, 3.747395293195558847E-16 ) ) ;
#3727 = CARTESIAN_POINT ( 'NONE',  ( 6.689389171169558779, -4.795626085247174153, 6.857782953271941950E-17 ) ) ;
#3728 = AXIS2_PLACEMENT_3D ( 'NONE', #1278, #3180, #7885 ) ;
#3729 = DIRECTION ( 'NONE',  ( 0.000000000000000000, 0.6691306063588593478, -0.7431448254773931339 ) ) ;
#3730 = ORIENTED_EDGE ( 'NONE', *, *, #973, .T. ) ;
#3731 = ORIENTED_EDGE ( 'NONE', *, *, #4086, .T. ) ;
#3732 = CARTESIAN_POINT ( 'NONE',  ( 1.500000000000000444, 19.43515443678402832, 15.40502424595151787 ) ) ;
#3733 = EDGE_LOOP ( 'NONE', ( #4737, #1879, #5475, #540 ) ) ;
#3734 = AXIS2_PLACEMENT_3D ( 'NONE', #7248, #10934, #8244 ) ;
#3735 = ORIENTED_EDGE ( 'NONE', *, *, #1989, .T. ) ;
#3736 = CARTESIAN_POINT ( 'NONE',  ( 0.000000000000000000, 0.000000000000000000, 0.000000000000000000 ) ) ;
#3737 = AXIS2_PLACEMENT_3D ( 'NONE', #9733, #3131, #7592 ) ;
#3738 = CARTESIAN_POINT ( 'NONE',  ( 3.000000000000000888, -5.135568396240178579, 21.96011696265489377 ) ) ;
#3739 = EDGE_CURVE ( 'NONE', #8566, #4413, #2270, .T. ) ;
#3740 = ORIENTED_EDGE ( 'NONE', *, *, #6602, .T. ) ;
#3741 = ADVANCED_FACE ( 'NONE', ( #7840 ), #125, .T. ) ;
#3742 = CARTESIAN_POINT ( 'NONE',  ( 0.000000000000000000, 11.67026512804572924, -19.29833442572348190 ) ) ;
#3743 = LINE ( 'NONE', #4903, #6301 ) ;
#3744 = CARTESIAN_POINT ( 'NONE',  ( -13.43906451854462603, -9.301052350413224090, 6.857782953271941950E-17 ) ) ;
#3745 = CIRCLE ( 'NONE', #4106, 9.599999999999997868 ) ;
#3746 = DIRECTION ( 'NONE',  ( 0.000000000000000000, 0.000000000000000000, 1.000000000000000000 ) ) ;
#3747 = CIRCLE ( 'NONE', #10189, 22.99899999999999523 ) ;
#3748 = CIRCLE ( 'NONE', #5310, 9.599999999999996092 ) ;
#3749 = DIRECTION ( 'NONE',  ( -1.000000000000000000, 0.000000000000000000, 0.000000000000000000 ) ) ;
#3750 = VERTEX_POINT ( 'NONE', #309 ) ;
#3751 = ORIENTED_EDGE ( 'NONE', *, *, #10417, .T. ) ;
#3752 = FACE_OUTER_BOUND ( 'NONE', #7373, .T. ) ;
#3753 = ORIENTED_EDGE ( 'NONE', *, *, #7434, .F. ) ;
#3754 = EDGE_CURVE ( 'NONE', #3183, #11249, #2033, .T. ) ;
#3755 = CARTESIAN_POINT ( 'NONE',  ( 15.00667705184754119, -6.512453894250635145, 10.00000000000000000 ) ) ;
#3756 = EDGE_CURVE ( 'NONE', #8232, #845, #1182, .T. ) ;
#3757 = AXIS2_PLACEMENT_3D ( 'NONE', #5217, #4293, #11762 ) ;
#3758 = CARTESIAN_POINT ( 'NONE',  ( 3.000000000000000888, -22.47229024614976112, -1.901833551798492561 ) ) ;
#3759 = ORIENTED_EDGE ( 'NONE', *, *, #4122, .F. ) ;
#3760 = AXIS2_PLACEMENT_3D ( 'NONE', #9170, #786, #6541 ) ;
#3761 = DIRECTION ( 'NONE',  ( 0.000000000000000000, 0.000000000000000000, 1.000000000000000000 ) ) ;
#3762 = CYLINDRICAL_SURFACE ( 'NONE', #10837, 22.99899999999999878 ) ;
#3763 = CARTESIAN_POINT ( 'NONE',  ( -1.103316172498668202, -16.73802372459124754, 10.00000000000000000 ) ) ;
#3764 = CARTESIAN_POINT ( 'NONE',  ( 1.018538006779708738, -7.771884277300779686, 6.857782953271941950E-17 ) ) ;
#3765 = CYLINDRICAL_SURFACE ( 'NONE', #9443, 22.99899999999999878 ) ;
#3766 = VECTOR ( 'NONE', #6787, 1000.000000000000000 ) ;
#3767 = DIRECTION ( 'NONE',  ( -1.000000000000000000, 0.000000000000000000, 0.000000000000000000 ) ) ;
#3768 = AXIS2_PLACEMENT_3D ( 'NONE', #11272, #1845, #3923 ) ;
#3769 = ORIENTED_EDGE ( 'NONE', *, *, #2550, .F. ) ;
#3770 = ORIENTED_EDGE ( 'NONE', *, *, #7618, .T. ) ;
#3771 = EDGE_CURVE ( 'NONE', #11767, #9480, #10764, .T. ) ;
#3772 = ORIENTED_EDGE ( 'NONE', *, *, #7122, .T. ) ;
#3773 = CARTESIAN_POINT ( 'NONE',  ( 0.000000000000000000, 15.42759117534385993, 16.45023496161670451 ) ) ;
#3774 = CARTESIAN_POINT ( 'NONE',  ( 1.831757423467613277, 7.960349185506228942, 10.00000000000000000 ) ) ;
#3775 = CARTESIAN_POINT ( 'NONE',  ( 3.000000000000000888, 21.96011696265491153, -5.135568396240103084 ) ) ;
#3776 = AXIS2_PLACEMENT_3D ( 'NONE', #6403, #11185, #10131 ) ;
#3777 = DIRECTION ( 'NONE',  ( 0.000000000000000000, 0.000000000000000000, 1.000000000000000000 ) ) ;
#3778 = FACE_OUTER_BOUND ( 'NONE', #5365, .T. ) ;
#3779 = CARTESIAN_POINT ( 'NONE',  ( -8.962830026514755133, 0.7152994853347065529, 3.747395293195558847E-16 ) ) ;
#3780 = AXIS2_PLACEMENT_3D ( 'NONE', #2969, #13, #1011 ) ;
#3781 = CARTESIAN_POINT ( 'NONE',  ( 3.000000000000000888, 11.20082935824103387, -20.08719549084852929 ) ) ;
#3782 = DIRECTION ( 'NONE',  ( -1.000000000000000000, -0.000000000000000000, 0.000000000000000000 ) ) ;
#3783 = ORIENTED_EDGE ( 'NONE', *, *, #7362, .F. ) ;
#3784 = EDGE_CURVE ( 'NONE', #1833, #11632, #5772, .T. ) ;
#3785 = ORIENTED_EDGE ( 'NONE', *, *, #5734, .F. ) ;
#3786 = CIRCLE ( 'NONE', #10617, 9.599999999999997868 ) ;
#3787 = VERTEX_POINT ( 'NONE', #10597 ) ;
#3788 = ORIENTED_EDGE ( 'NONE', *, *, #10467, .T. ) ;
#3789 = DIRECTION ( 'NONE',  ( 0.000000000000000000, -0.7431448254773999063, 0.6691306063588520203 ) ) ;
#3790 = CARTESIAN_POINT ( 'NONE',  ( 3.000000000000000888, -15.64281154287608722, 16.85990652506894705 ) ) ;
#3791 = DIRECTION ( 'NONE',  ( 0.000000000000000000, 0.000000000000000000, 1.000000000000000000 ) ) ;
#3792 = CARTESIAN_POINT ( 'NONE',  ( 0.000000000000000000, 0.000000000000000000, 10.00000000000000000 ) ) ;
#3793 = EDGE_CURVE ( 'NONE', #6911, #3296, #5699, .T. ) ;
#3794 = CIRCLE ( 'NONE', #9458, 22.99899999999999878 ) ;
#3795 = CARTESIAN_POINT ( 'NONE',  ( 3.000000000000000888, 0.000000000000000000, 0.000000000000000000 ) ) ;
#3796 = CARTESIAN_POINT ( 'NONE',  ( 12.15471013770256903, -5.500887282572993975, 3.747395293195558847E-16 ) ) ;
#3797 = CARTESIAN_POINT ( 'NONE',  ( 0.000000000000000000, -10.87771529938174808, 19.75591328264882662 ) ) ;
#3798 = DIRECTION ( 'NONE',  ( 0.000000000000000000, 0.000000000000000000, 1.000000000000000000 ) ) ;
#3799 = ORIENTED_EDGE ( 'NONE', *, *, #1950, .F. ) ;
#3800 = ORIENTED_EDGE ( 'NONE', *, *, #1943, .T. ) ;
#3801 = DIRECTION ( 'NONE',  ( 0.000000000000000000, 0.3090169943749416781, 0.9510565162951555296 ) ) ;
#3802 = ORIENTED_EDGE ( 'NONE', *, *, #8349, .T. ) ;
#3803 = CIRCLE ( 'NONE', #4382, 9.599999999999996092 ) ;
#3804 = DIRECTION ( 'NONE',  ( -1.000000000000000000, 0.000000000000000000, 0.000000000000000000 ) ) ;
#3805 = CARTESIAN_POINT ( 'NONE',  ( 3.000000000000000888, 0.000000000000000000, 0.000000000000000000 ) ) ;
#3806 = ORIENTED_EDGE ( 'NONE', *, *, #8383, .T. ) ;
#3807 = DIRECTION ( 'NONE',  ( -1.000000000000000000, -0.000000000000000000, 0.000000000000000000 ) ) ;
#3808 = DIRECTION ( 'NONE',  ( -1.000000000000000000, 0.000000000000000000, 0.000000000000000000 ) ) ;
#3809 = CARTESIAN_POINT ( 'NONE',  ( 5.531377455021724288, -0.3672033614207039776, 10.00000000000000000 ) ) ;
#3810 = CIRCLE ( 'NONE', #7303, 9.599999999999996092 ) ;
#3811 = FACE_OUTER_BOUND ( 'NONE', #6615, .T. ) ;
#3812 = LINE ( 'NONE', #5584, #2166 ) ;
#3813 = ORIENTED_EDGE ( 'NONE', *, *, #837, .F. ) ;
#3814 = ORIENTED_EDGE ( 'NONE', *, *, #242, .F. ) ;
#3815 = DIRECTION ( 'NONE',  ( 1.000000000000000000, -0.000000000000000000, 0.000000000000000000 ) ) ;
#3816 = EDGE_LOOP ( 'NONE', ( #306, #4188, #5544, #8713 ) ) ;
#3817 = CARTESIAN_POINT ( 'NONE',  ( 11.72652038055310086, 7.297668919378235586, 10.00000000000000000 ) ) ;
#3818 = CARTESIAN_POINT ( 'NONE',  ( 0.0002901587068756704066, -4.749354241797638210, 6.857782953271941950E-17 ) ) ;
#3819 = ORIENTED_EDGE ( 'NONE', *, *, #7152, .T. ) ;
#3820 = DIRECTION ( 'NONE',  ( -1.000000000000000000, -0.000000000000000000, 0.000000000000000000 ) ) ;
#3821 = DIRECTION ( 'NONE',  ( -1.000000000000000000, -0.000000000000000000, 0.000000000000000000 ) ) ;
#3822 = CARTESIAN_POINT ( 'NONE',  ( -9.080917052262543976, 12.68274194616037853, 10.00000000000000000 ) ) ;
#3823 = PRODUCT_RELATED_PRODUCT_CATEGORY ( 'part', '', ( #6001 ) ) ;
#3824 = CARTESIAN_POINT ( 'NONE',  ( 0.000000000000000000, 0.000000000000000000, 0.000000000000000000 ) ) ;
#3825 = DIRECTION ( 'NONE',  ( 0.000000000000000000, 0.9781476007338049117, 0.2079116908177629230 ) ) ;
#3826 = ADVANCED_FACE ( 'NONE', ( #6677 ), #1112, .T. ) ;
#3827 = CYLINDRICAL_SURFACE ( 'NONE', #7446, 22.99899999999999878 ) ;
#3828 = ORIENTED_EDGE ( 'NONE', *, *, #8724, .F. ) ;
#3829 = AXIS2_PLACEMENT_3D ( 'NONE', #4426, #1673, #10979 ) ;
#3830 = EDGE_CURVE ( 'NONE', #6334, #3911, #3547, .T. ) ;
#3831 = DIRECTION ( 'NONE',  ( -0.000000000000000000, -0.000000000000000000, -1.000000000000000000 ) ) ;
#3832 = ORIENTED_EDGE ( 'NONE', *, *, #4942, .T. ) ;
#3833 = DIRECTION ( 'NONE',  ( 1.000000000000000000, 0.000000000000000000, 0.000000000000000000 ) ) ;
#3834 = CARTESIAN_POINT ( 'NONE',  ( -9.037587479195734019, -0.7561632655184234997, 10.00000000000000000 ) ) ;
#3835 = DIRECTION ( 'NONE',  ( -1.000000000000000000, -0.000000000000000000, -0.000000000000000000 ) ) ;
#3836 = AXIS2_PLACEMENT_3D ( 'NONE', #8018, #6069, #493 ) ;
#3837 = CARTESIAN_POINT ( 'NONE',  ( -5.920784292472551336, 6.290491683487165808, 3.747395293195558847E-16 ) ) ;
#3838 = CARTESIAN_POINT ( 'NONE',  ( 0.3190826481552654914, -3.778307095988950870, 3.747395293195558847E-16 ) ) ;
#3839 = DIRECTION ( 'NONE',  ( 0.000000000000000000, 0.000000000000000000, 1.000000000000000000 ) ) ;
#3840 = ORIENTED_EDGE ( 'NONE', *, *, #10173, .T. ) ;
#3841 = EDGE_LOOP ( 'NONE', ( #6346, #4911, #10708, #564 ) ) ;
#3842 = AXIS2_PLACEMENT_3D ( 'NONE', #479, #7763, #7827 ) ;
#3843 = ORIENTED_EDGE ( 'NONE', *, *, #11376, .F. ) ;
#3844 = DIRECTION ( 'NONE',  ( 1.000000000000000000, 0.000000000000000000, 0.000000000000000000 ) ) ;
#3845 = ADVANCED_FACE ( 'NONE', ( #5080 ), #7145, .T. ) ;
#3846 = DIRECTION ( 'NONE',  ( -1.000000000000000000, 0.000000000000000000, 0.000000000000000000 ) ) ;
#3847 = CARTESIAN_POINT ( 'NONE',  ( 3.000000000000000888, -22.90635393027944744, -2.062268319295799568 ) ) ;
#3848 = DIRECTION ( 'NONE',  ( -1.000000000000000000, 0.000000000000000000, 0.000000000000000000 ) ) ;
#3849 = EDGE_CURVE ( 'NONE', #4270, #10729, #2389, .T. ) ;
#3850 = DIRECTION ( 'NONE',  ( 1.000000000000000000, 0.000000000000000000, 0.000000000000000000 ) ) ;
#3851 = CARTESIAN_POINT ( 'NONE',  ( 6.600721363681633314, -14.58171973507987396, 3.747395293195558847E-16 ) ) ;
#3852 = CARTESIAN_POINT ( 'NONE',  ( 8.000000000000000000, 0.000000000000000000, 19.99999999999999645 ) ) ;
#3853 = ORIENTED_EDGE ( 'NONE', *, *, #9086, .F. ) ;
#3854 = ORIENTED_EDGE ( 'NONE', *, *, #442, .F. ) ;
#3855 = CYLINDRICAL_SURFACE ( 'NONE', #11566, 24.80000000000000071 ) ;
#3856 = EDGE_CURVE ( 'NONE', #11027, #3033, #1006, .T. ) ;
#3857 = EDGE_LOOP ( 'NONE', ( #10674, #1620, #1188, #2691 ) ) ;
#3858 = DIRECTION ( 'NONE',  ( 0.000000000000000000, 0.000000000000000000, -1.000000000000000000 ) ) ;
#3859 = DIRECTION ( 'NONE',  ( 0.000000000000000000, 0.000000000000000000, 1.000000000000000000 ) ) ;
#3860 = ORIENTED_EDGE ( 'NONE', *, *, #7341, .T. ) ;
#3861 = DIRECTION ( 'NONE',  ( -1.000000000000000000, 0.000000000000000000, 0.000000000000000000 ) ) ;
#3862 = CARTESIAN_POINT ( 'NONE',  ( 0.000000000000000000, 13.28910708463128287, 20.93895013827586382 ) ) ;
#3863 = CARTESIAN_POINT ( 'NONE',  ( -8.799721882313772170, 9.100398320382241835, 6.857782953271941950E-17 ) ) ;
#3864 = CARTESIAN_POINT ( 'NONE',  ( 0.000000000000000000, 0.000000000000000000, 0.000000000000000000 ) ) ;
#3865 = DIRECTION ( 'NONE',  ( 0.000000000000000000, 0.000000000000000000, 1.000000000000000000 ) ) ;
#3866 = CIRCLE ( 'NONE', #1932, 24.80000000000000071 ) ;
#3867 = ORIENTED_EDGE ( 'NONE', *, *, #11999, .F. ) ;
#3868 = ORIENTED_EDGE ( 'NONE', *, *, #7012, .F. ) ;
#3869 = DIRECTION ( 'NONE',  ( -1.000000000000000000, -0.000000000000000000, -0.000000000000000000 ) ) ;
#3870 = VERTEX_POINT ( 'NONE', #7086 ) ;
#3871 = CARTESIAN_POINT ( 'NONE',  ( -14.60057116351880069, -4.165219547604622541, 10.00000000000000000 ) ) ;
#3872 = DIRECTION ( 'NONE',  ( -1.000000000000000000, 0.000000000000000000, 0.000000000000000000 ) ) ;
#3873 =( LENGTH_UNIT ( ) NAMED_UNIT ( * ) SI_UNIT ( .MILLI., .METRE. ) );
#3874 = APPLICATION_CONTEXT ( 'automotive_design' ) ;
#3875 = CIRCLE ( 'NONE', #2899, 24.80000000000000071 ) ;
#3876 = DIRECTION ( 'NONE',  ( -1.000000000000000000, -0.000000000000000000, -0.000000000000000000 ) ) ;
#3877 = DIRECTION ( 'NONE',  ( 0.000000000000000000, -0.9781476007338077983, 0.2079116908177493783 ) ) ;
#3878 = CARTESIAN_POINT ( 'NONE',  ( 4.451863640886955409, 11.26298505921346305, 10.00000000000000000 ) ) ;
#3879 = DIRECTION ( 'NONE',  ( -1.000000000000000000, -0.000000000000000000, 0.000000000000000000 ) ) ;
#3880 = DIRECTION ( 'NONE',  ( -0.000000000000000000, -0.000000000000000000, 1.000000000000000000 ) ) ;
#3881 = VERTEX_POINT ( 'NONE', #11631 ) ;
#3882 = LINE ( 'NONE', #1639, #6262 ) ;
#3883 = VECTOR ( 'NONE', #5060, 1000.000000000000000 ) ;
#3884 = CIRCLE ( 'NONE', #158, 22.99899999999999523 ) ;
#3885 = EDGE_LOOP ( 'NONE', ( #6021, #9486, #3375, #11038 ) ) ;
#3886 = DIRECTION ( 'NONE',  ( 0.000000000000000000, 0.000000000000000000, 1.000000000000000000 ) ) ;
#3887 = CARTESIAN_POINT ( 'NONE',  ( 6.685168693379562654, -7.607270790100137958, 10.00000000000000000 ) ) ;
#3888 = EDGE_CURVE ( 'NONE', #7388, #9445, #6855, .T. ) ;
#3889 = DIRECTION ( 'NONE',  ( 0.000000000000000000, 0.000000000000000000, 1.000000000000000000 ) ) ;
#3890 = EDGE_CURVE ( 'NONE', #3469, #2524, #1349, .T. ) ;
#3891 = CARTESIAN_POINT ( 'NONE',  ( 0.5199114366211738947, 8.229807867079655281, 3.747395293195558847E-16 ) ) ;
#3892 = CIRCLE ( 'NONE', #553, 1.500000000000000222 ) ;
#3893 = CARTESIAN_POINT ( 'NONE',  ( 14.22875512193218661, -2.589574901423981057, 6.857782953271941950E-17 ) ) ;
#3894 = CARTESIAN_POINT ( 'NONE',  ( 1.499999999999999556, 23.88662356770115380, 6.668524164681708832 ) ) ;
#3895 = VERTEX_POINT ( 'NONE', #8940 ) ;
#3896 = VERTEX_POINT ( 'NONE', #6128 ) ;
#3898 = EDGE_CURVE ( 'NONE', #5856, #2132, #4282, .T. ) ;
#3897 = CIRCLE ( 'NONE', #5459, 22.99899999999999878 ) ;
#3899 = DIRECTION ( 'NONE',  ( -1.000000000000000000, -0.000000000000000000, 0.000000000000000000 ) ) ;
#3900 = AXIS2_PLACEMENT_3D ( 'NONE', #11672, #12081, #1459 ) ;
#3901 = DIRECTION ( 'NONE',  ( -1.000000000000000000, 0.000000000000000000, -0.000000000000000000 ) ) ;
#3902 = ORIENTED_EDGE ( 'NONE', *, *, #619, .T. ) ;
#3903 = CARTESIAN_POINT ( 'NONE',  ( 3.000000000000000888, -13.72351598154883412, -20.65684170206505144 ) ) ;
#3904 = FACE_OUTER_BOUND ( 'NONE', #182, .T. ) ;
#3905 = CARTESIAN_POINT ( 'NONE',  ( 3.000000000000000888, 0.000000000000000000, 0.000000000000000000 ) ) ;
#3906 = CARTESIAN_POINT ( 'NONE',  ( -14.61026919807147095, 3.159152207411756397, 3.747395293195558847E-16 ) ) ;
#3907 = AXIS2_PLACEMENT_3D ( 'NONE', #4821, #3846, #3658 ) ;
#3908 = EDGE_CURVE ( 'NONE', #7759, #9316, #10380, .T. ) ;
#3909 = AXIS2_PLACEMENT_3D ( 'NONE', #774, #11970, #11059 ) ;
#3910 = DIRECTION ( 'NONE',  ( 1.445602896647338917E-16, -1.000000000000000000, 0.000000000000000000 ) ) ;
#3911 = VERTEX_POINT ( 'NONE', #2508 ) ;
#3912 = EDGE_LOOP ( 'NONE', ( #10953, #2566, #4128, #3645 ) ) ;
#3913 = DIRECTION ( 'NONE',  ( -1.000000000000000000, -0.000000000000000000, -0.000000000000000000 ) ) ;
#3914 = ORIENTED_EDGE ( 'NONE', *, *, #10856, .F. ) ;
#3915 = ADVANCED_FACE ( 'NONE', ( #1595 ), #4172, .T. ) ;
#3916 = CARTESIAN_POINT ( 'NONE',  ( 1.445324715877977173, -3.701599742324200637, 10.00000000000000000 ) ) ;
#3917 = CIRCLE ( 'NONE', #1570, 11.50000000000000178 ) ;
#3918 = DIRECTION ( 'NONE',  ( 0.000000000000000000, 0.9781476007338062439, -0.2079116908177564282 ) ) ;
#3919 = ORIENTED_EDGE ( 'NONE', *, *, #4936, .F. ) ;
#3920 = CIRCLE ( 'NONE', #4900, 24.80000000000000071 ) ;
#3921 = DIRECTION ( 'NONE',  ( 0.000000000000000000, 0.000000000000000000, 1.000000000000000000 ) ) ;
#3922 = PRODUCT_DEFINITION_FORMATION_WITH_SPECIFIED_SOURCE ( 'ANY', '', #2185, .NOT_KNOWN. ) ;
#3923 = DIRECTION ( 'NONE',  ( 1.000000000000000000, 0.000000000000000000, 0.000000000000000000 ) ) ;
#3924 = CARTESIAN_POINT ( 'NONE',  ( 13.14573027368987646, 6.745762002080606834, 6.857782953271941950E-17 ) ) ;
#3925 = PLANE ( 'NONE',  #2365 ) ;
#3926 = CIRCLE ( 'NONE', #6267, 22.99899999999999523 ) ;
#3927 = FACE_OUTER_BOUND ( 'NONE', #12030, .T. ) ;
#3928 = ORIENTED_EDGE ( 'NONE', *, *, #8349, .F. ) ;
#3929 = CIRCLE ( 'NONE', #1381, 9.599999999999994316 ) ;
#3930 = ORIENTED_EDGE ( 'NONE', *, *, #7237, .T. ) ;
#3931 = DIRECTION ( 'NONE',  ( 0.000000000000000000, 0.000000000000000000, 1.000000000000000000 ) ) ;
#3932 = VERTEX_POINT ( 'NONE', #8997 ) ;
#3933 = ADVANCED_FACE ( 'NONE', ( #9971 ), #5333, .T. ) ;
#3934 = AXIS2_PLACEMENT_3D ( 'NONE', #9540, #7703, #3058 ) ;
#3935 = CARTESIAN_POINT ( 'NONE',  ( 7.081399987883182590, -10.98142027556026967, 10.00000000000000000 ) ) ;
#3936 = DIRECTION ( 'NONE',  ( -1.000000000000000000, 0.000000000000000000, 0.000000000000000000 ) ) ;
#3937 =( NAMED_UNIT ( * ) PLANE_ANGLE_UNIT ( ) SI_UNIT ( $, .RADIAN. ) );
#3938 = AXIS2_PLACEMENT_3D ( 'NONE', #4608, #3684, #929 ) ;
#3940 = AXIS2_PLACEMENT_3D ( 'NONE', #3864, #7587, #11328 ) ;
#3939 = DIRECTION ( 'NONE',  ( 0.000000000000000000, 0.9945218953682729568, 0.1045284632676571068 ) ) ;
#3941 = ADVANCED_FACE ( 'NONE', ( #488 ), #4405, .T. ) ;
#3942 = AXIS2_PLACEMENT_3D ( 'NONE', #6626, #4491, #6448 ) ;
#3943 = FACE_OUTER_BOUND ( 'NONE', #4640, .T. ) ;
#3944 = CARTESIAN_POINT ( 'NONE',  ( -12.98359546555290045, 0.8565524458112724338, 10.00000000000000000 ) ) ;
#3945 = DIRECTION ( 'NONE',  ( 0.000000000000000000, 0.000000000000000000, 1.000000000000000000 ) ) ;
#3946 = CARTESIAN_POINT ( 'NONE',  ( 3.000000000000000888, -18.80635025205160815, -13.23915371906974592 ) ) ;
#3947 = CARTESIAN_POINT ( 'NONE',  ( 3.000000000000002665, 0.000000000000000000, 4.000000000000000000 ) ) ;
#3948 = DIRECTION ( 'NONE',  ( 0.000000000000000000, 0.000000000000000000, -1.000000000000000000 ) ) ;
#3949 = CLOSED_SHELL ( 'NONE', ( #7768, #1676, #489, #3382, #1308, #2501, #1540, #10342, #8766, #1651, #10012, #8717, #3970, #6099, #7160, #1897, #6384, #7665, #3626, #4163, #4562, #6517, #7725, #6022, #8619, #11565, #7488, #4433, #4746, #2245, #2800, #8026, #6056, #5576, #11092, #3915, #3027, #4591, #9234, #2068, #5911, #6943, #678, #3046, #9696, #9385, #6443, #5171, #11445, #7510, #6428, #9574, #3477, #4009, #8309, #9062, #11598, #3741, #405, #11187, #5636, #3081, #9049, #9324, #10405, #1732, #2106, #3591, #2243, #10313, #6365, #8978, #1874, #4907, #527, #11000, #9308, #2857, #6280, #5539, #11468, #247, #12115, #287, #10723, #3635, #3284, #1277, #285, #8222, #8339, #7617, #10161, #4295, #4573, #928, #4638, #7106, #1513, #8184, #7501, #7545, #7579, #11160, #7612, #11657, #1014, #4303, #9883, #11736, #9391, #11251, #4050, #11666, #1868, #10480, #1610, #445, #4457, #2200, #6725, #2697, #6083, #1750, #10099, #3826, #6387, #7324, #5806, #6244, #10542, #138, #11472, #6877, #11143, #8146, #397, #10194, #7177, #3278, #9206, #7925, #106, #1891, #5115, #9724, #69, #3317, #3398, #6537, #11858, #7473, #2916, #9671, #10500, #5652, #3368, #10634, #10944, #9851, #4380, #373, #780, #1363, #10017, #6840, #11083, #6361, #7623, #7654, #5424, #8300, #7524, #7382, #9014, #9581, #5123, #1384, #7088, #1136, #1192, #9464, #735, #3377, #2036, #3310, #4449, #907, #2392, #5910, #5985, #9968, #3941, #2093, #7996, #7476, #10929, #8089, #6965, #1949, #1461, #10731, #1339, #6596, #7776, #6220, #93, #10858, #8875, #5392, #24, #6793, #5021, #517, #4789, #3197, #3845, #4041, #9156, #9940, #5085, #1083, #6961, #3960, #1296, #9311, #2208, #10421, #2889, #6694, #986, #521, #8900, #3602, #1196, #1504, #1805, #4495, #10545, #11827, #3933, #2682, #8570, #5776, #4751, #11834, #8633, #8437, #8608, #11069, #5864, #2170, #2135, #7892, #5006 ) ) ;
#3950 = ORIENTED_EDGE ( 'NONE', *, *, #8120, .T. ) ;
#3951 = EDGE_LOOP ( 'NONE', ( #3588, #10076, #11009, #2877 ) ) ;
#3952 = DIRECTION ( 'NONE',  ( -1.000000000000000000, 0.000000000000000000, -0.000000000000000000 ) ) ;
#3953 = CARTESIAN_POINT ( 'NONE',  ( -1.790740696106539520, -6.394195405909708363, 10.00000000000000000 ) ) ;
#3954 = CYLINDRICAL_SURFACE ( 'NONE', #9553, 9.599999999999997868 ) ;
#3955 = CARTESIAN_POINT ( 'NONE',  ( 8.143984375790578767, 3.063465613658708619, 10.00000000000000000 ) ) ;
#3956 = AXIS2_PLACEMENT_3D ( 'NONE', #3298, #6962, #5140 ) ;
#3957 = CARTESIAN_POINT ( 'NONE',  ( -12.91830213043053988, -2.344901317288421883, 6.857782953271941950E-17 ) ) ;
#3958 = LINE ( 'NONE', #5974, #1988 ) ;
#3959 = VERTEX_POINT ( 'NONE', #9913 ) ;
#3960 = ADVANCED_FACE ( 'NONE', ( #7899 ), #6968, .T. ) ;
#3961 = ORIENTED_EDGE ( 'NONE', *, *, #7874, .F. ) ;
#3962 = FACE_OUTER_BOUND ( 'NONE', #9270, .T. ) ;
#3963 = CARTESIAN_POINT ( 'NONE',  ( 3.000000000000000888, -9.039786367038983528, 21.14796121233193560 ) ) ;
#3964 = VERTEX_POINT ( 'NONE', #8139 ) ;
#3965 = EDGE_CURVE ( 'NONE', #2073, #6153, #7439, .T. ) ;
#3966 = DIRECTION ( 'NONE',  ( 0.000000000000000000, 0.000000000000000000, 1.000000000000000000 ) ) ;
#3967 = CARTESIAN_POINT ( 'NONE',  ( 3.000000000000000888, 7.432877647175206270, 21.76479567747243848 ) ) ;
#3968 = CARTESIAN_POINT ( 'NONE',  ( 1.499999999999999556, 24.02068490260621303, -6.168200451485523317 ) ) ;
#3969 = CARTESIAN_POINT ( 'NONE',  ( -11.98301361336074145, 0.7816210414391653316, 3.747395293195558847E-16 ) ) ;
#3970 = ADVANCED_FACE ( 'NONE', ( #2575 ), #6312, .T. ) ;
#3971 = AXIS2_PLACEMENT_3D ( 'NONE', #4167, #3189, #10590 ) ;
#3972 = EDGE_CURVE ( 'NONE', #3644, #4775, #10775, .T. ) ;
#3973 = DIRECTION ( 'NONE',  ( 0.000000000000000000, -0.1045284632676401482, -0.9945218953682747332 ) ) ;
#3974 = ORIENTED_EDGE ( 'NONE', *, *, #4108, .F. ) ;
#3975 = VECTOR ( 'NONE', #7999, 1000.000000000000000 ) ;
#3976 = VERTEX_POINT ( 'NONE', #1769 ) ;
#3977 = AXIS2_PLACEMENT_3D ( 'NONE', #193, #7670, #441 ) ;
#3978 = EDGE_CURVE ( 'NONE', #1804, #5933, #2634, .T. ) ;
#3979 = CARTESIAN_POINT ( 'NONE',  ( -11.98007164540817371, 10.17225797950328214, 10.00000000000000000 ) ) ;
#3980 = ORIENTED_EDGE ( 'NONE', *, *, #2664, .T. ) ;
#3981 = DIRECTION ( 'NONE',  ( -1.000000000000000000, 0.000000000000000000, 0.000000000000000000 ) ) ;
#3982 = CARTESIAN_POINT ( 'NONE',  ( 1.500000000000000444, -24.02068490260608868, -6.168200451486004710 ) ) ;
#3983 = AXIS2_PLACEMENT_3D ( 'NONE', #4588, #968, #8256 ) ;
#3984 = CARTESIAN_POINT ( 'NONE',  ( -1.500000000000000222, 1.836970198721030181E-16, -15.00000000000000000 ) ) ;
#3985 = ORIENTED_EDGE ( 'NONE', *, *, #1644, .T. ) ;
#3986 = DIRECTION ( 'NONE',  ( -1.000000000000000000, -0.000000000000000000, 0.000000000000000000 ) ) ;
#3987 = DIRECTION ( 'NONE',  ( -1.000000000000000000, -0.000000000000000000, 0.000000000000000000 ) ) ;
#3988 = CARTESIAN_POINT ( 'NONE',  ( -8.211874628637438889, -10.69266484962706087, 6.857782953271941950E-17 ) ) ;
#3989 = DIRECTION ( 'NONE',  ( 0.000000000000000000, 0.000000000000000000, 1.000000000000000000 ) ) ;
#3990 = ORIENTED_EDGE ( 'NONE', *, *, #9579, .F. ) ;
#3991 = CYLINDRICAL_SURFACE ( 'NONE', #9791, 1.500000000000000222 ) ;
#3992 = AXIS2_PLACEMENT_3D ( 'NONE', #3905, #11373, #6209 ) ;
#3993 = ORIENTED_EDGE ( 'NONE', *, *, #5734, .T. ) ;
#3994 = LINE ( 'NONE', #4105, #8614 ) ;
#3995 = VERTEX_POINT ( 'NONE', #1656 ) ;
#3996 = CARTESIAN_POINT ( 'NONE',  ( -14.24631147015002242, -5.364320868108786833, 10.00000000000000000 ) ) ;
#3997 = CYLINDRICAL_SURFACE ( 'NONE', #7537, 22.99899999999999878 ) ;
#3998 = CIRCLE ( 'NONE', #4387, 22.99899999999999878 ) ;
#3999 = CARTESIAN_POINT ( 'NONE',  ( 0.000000000000000000, 0.000000000000000000, 0.000000000000000000 ) ) ;
#4000 = CARTESIAN_POINT ( 'NONE',  ( 0.000000000000000000, 0.000000000000000000, 0.000000000000000000 ) ) ;
#4001 = CARTESIAN_POINT ( 'NONE',  ( 11.51680056346192593, -0.3781118375584788249, 10.00000000000000000 ) ) ;
#4002 = EDGE_CURVE ( 'NONE', #10066, #3234, #3342, .T. ) ;
#4003 = CARTESIAN_POINT ( 'NONE',  ( -8.207979594962566239, -13.19054478262514252, 3.747395293195558847E-16 ) ) ;
#4004 = CYLINDRICAL_SURFACE ( 'NONE', #8423, 19.99999999999999645 ) ;
#4005 = ORIENTED_EDGE ( 'NONE', *, *, #8252, .T. ) ;
#4006 = CARTESIAN_POINT ( 'NONE',  ( 3.000000000000000888, -2.811977935937640005, -22.37663021667346896 ) ) ;
#4007 = AXIS2_PLACEMENT_3D ( 'NONE', #4605, #9180, #5275 ) ;
#4008 = ORIENTED_EDGE ( 'NONE', *, *, #8682, .F. ) ;
#4009 = ADVANCED_FACE ( 'NONE', ( #4532 ), #8388, .T. ) ;
#4010 = ORIENTED_EDGE ( 'NONE', *, *, #9125, .T. ) ;
#4011 = CARTESIAN_POINT ( 'NONE',  ( 3.000000000000000888, -2.745295967525840375, -22.83456483164691875 ) ) ;
#4012 = CARTESIAN_POINT ( 'NONE',  ( -3.663109177303994546, -5.348850660921632638, 10.00000000000000000 ) ) ;
#4013 = CARTESIAN_POINT ( 'NONE',  ( 3.000000000000000888, -22.37663021667341923, -2.811977935938010376 ) ) ;
#4014 = CARTESIAN_POINT ( 'NONE',  ( 10.63538685525201188, -4.008487272325480966, 10.00000000000000000 ) ) ;
#4015 = CARTESIAN_POINT ( 'NONE',  ( 12.58137556868280882, 7.823023050434559700, 6.857782953271941950E-17 ) ) ;
#4016 = SURFACE_STYLE_USAGE ( .BOTH. , #8789 ) ;
#4017 = LINE ( 'NONE', #7743, #5112 ) ;
#4018 = VERTEX_POINT ( 'NONE', #10222 ) ;
#4019 = ORIENTED_EDGE ( 'NONE', *, *, #4189, .F. ) ;
#4020 = CARTESIAN_POINT ( 'NONE',  ( -10.00000000000000000, 0.000000000000000000, 0.000000000000000000 ) ) ;
#4021 = CARTESIAN_POINT ( 'NONE',  ( 0.000000000000000000, 22.90635393027949007, -2.062268319295327057 ) ) ;
#4022 = DIRECTION ( 'NONE',  ( -1.000000000000000000, -0.000000000000000000, -0.000000000000000000 ) ) ;
#4023 = FACE_OUTER_BOUND ( 'NONE', #3432, .T. ) ;
#4024 = CARTESIAN_POINT ( 'NONE',  ( 4.889075487039526990, 9.929493272050624597, 3.747395293195558847E-16 ) ) ;
#4025 = AXIS2_PLACEMENT_3D ( 'NONE', #1914, #10297, #11337 ) ;
#4026 = DIRECTION ( 'NONE',  ( -1.000000000000000000, 0.000000000000000000, 0.000000000000000000 ) ) ;
#4027 = ORIENTED_EDGE ( 'NONE', *, *, #4857, .T. ) ;
#4028 = ORIENTED_EDGE ( 'NONE', *, *, #4414, .F. ) ;
#4029 = CARTESIAN_POINT ( 'NONE',  ( 0.000000000000000000, 0.000000000000000000, 0.000000000000000000 ) ) ;
#4030 = CARTESIAN_POINT ( 'NONE',  ( -3.251399079312189855, 15.05603916236422890, 10.00000000000000000 ) ) ;
#4031 = ORIENTED_EDGE ( 'NONE', *, *, #9751, .T. ) ;
#4032 = LINE ( 'NONE', #7760, #10922 ) ;
#4033 = CARTESIAN_POINT ( 'NONE',  ( 0.000000000000000000, -24.02068490260608868, -6.168200451486004710 ) ) ;
#4034 = EDGE_CURVE ( 'NONE', #4410, #11830, #10089, .T. ) ;
#4035 = DIRECTION ( 'NONE',  ( 0.000000000000000000, -0.9135454576426046414, 0.4067366430757919926 ) ) ;
#4036 = AXIS2_PLACEMENT_3D ( 'NONE', #9070, #5515, #2581 ) ;
#4037 = EDGE_LOOP ( 'NONE', ( #7398, #6407, #4578, #5492 ) ) ;
#4038 = EDGE_CURVE ( 'NONE', #5213, #712, #4523, .T. ) ;
#4039 = DIRECTION ( 'NONE',  ( 0.000000000000000000, -0.3090169943749349613, -0.9510565162951576390 ) ) ;
#4040 = EDGE_CURVE ( 'NONE', #4720, #2635, #9197, .T. ) ;
#4041 = ADVANCED_FACE ( 'NONE', ( #11076 ), #5572, .T. ) ;
#4042 = CARTESIAN_POINT ( 'NONE',  ( 3.000000000000000888, 0.000000000000000000, 0.000000000000000000 ) ) ;
#4043 = CARTESIAN_POINT ( 'NONE',  ( 0.5005346673319864825, 15.27733729710887545, 6.857782953271941950E-17 ) ) ;
#4044 = ORIENTED_EDGE ( 'NONE', *, *, #5951, .T. ) ;
#4045 = CARTESIAN_POINT ( 'NONE',  ( -10.00000000000000000, 0.000000000000000000, 0.000000000000000000 ) ) ;
#4046 = ORIENTED_EDGE ( 'NONE', *, *, #11629, .F. ) ;
#4047 = DIRECTION ( 'NONE',  ( -1.000000000000000000, -0.000000000000000000, -0.000000000000000000 ) ) ;
#4048 = ORIENTED_EDGE ( 'NONE', *, *, #12012, .F. ) ;
#4049 = CARTESIAN_POINT ( 'NONE',  ( 5.319643049700913728, -8.526005966359200272, 10.00000000000000000 ) ) ;
#4050 = ADVANCED_FACE ( 'NONE', ( #6544 ), #10277, .T. ) ;
#4051 = PLANE ( 'NONE',  #8134 ) ;
#4052 = ORIENTED_EDGE ( 'NONE', *, *, #5614, .T. ) ;
#4053 = CARTESIAN_POINT ( 'NONE',  ( 0.000000000000000000, 0.000000000000000000, 0.000000000000000000 ) ) ;
#4054 = DIRECTION ( 'NONE',  ( 0.000000000000000000, 0.000000000000000000, 1.000000000000000000 ) ) ;
#4055 = CARTESIAN_POINT ( 'NONE',  ( 4.479449988082535583, -13.21383449271838550, 10.00000000000000000 ) ) ;
#4056 = CIRCLE ( 'NONE', #11899, 9.599999999999997868 ) ;
#4057 = FACE_OUTER_BOUND ( 'NONE', #6546, .T. ) ;
#4058 = CARTESIAN_POINT ( 'NONE',  ( -14.85975435031504510, 1.953672781916663936, 3.747395293195558847E-16 ) ) ;
#4059 = FACE_BOUND ( 'NONE', #9392, .T. ) ;
#4060 = EDGE_CURVE ( 'NONE', #2665, #7274, #11362, .T. ) ;
#4061 = CARTESIAN_POINT ( 'NONE',  ( 0.000000000000000000, 0.000000000000000000, 0.000000000000000000 ) ) ;
#4062 = ORIENTED_EDGE ( 'NONE', *, *, #1352, .T. ) ;
#4063 = EDGE_LOOP ( 'NONE', ( #8283, #9171, #3423, #11613 ) ) ;
#4064 = ORIENTED_EDGE ( 'NONE', *, *, #2759, .F. ) ;
#4065 = EDGE_CURVE ( 'NONE', #5179, #994, #6424, .T. ) ;
#4066 = CIRCLE ( 'NONE', #11300, 9.599999999999997868 ) ;
#4067 = CYLINDRICAL_SURFACE ( 'NONE', #7921, 9.599999999999997868 ) ;
#4068 = CARTESIAN_POINT ( 'NONE',  ( -3.231136241382285501, -5.666136714101813965, 10.00000000000000000 ) ) ;
#4069 = DIRECTION ( 'NONE',  ( -1.000000000000000000, 0.000000000000000000, -0.000000000000000000 ) ) ;
#4070 = CARTESIAN_POINT ( 'NONE',  ( 3.000000000000000888, -18.51065745848368849, -12.88318129270198042 ) ) ;
#4071 = CARTESIAN_POINT ( 'NONE',  ( 10.90031251054716499, 4.301772984117411269, 10.00000000000000000 ) ) ;
#4072 = CARTESIAN_POINT ( 'NONE',  ( -2.240087900411201982, -13.53314956822677928, 6.857782953271941950E-17 ) ) ;
#4073 =( NAMED_UNIT ( * ) SI_UNIT ( $, .STERADIAN. ) SOLID_ANGLE_UNIT ( ) );
#4074 = EDGE_CURVE ( 'NONE', #6153, #5028, #11354, .T. ) ;
#4075 = AXIS2_PLACEMENT_3D ( 'NONE', #10071, #10876, #3346 ) ;
#4076 = DIRECTION ( 'NONE',  ( -1.000000000000000000, 0.000000000000000000, 0.000000000000000000 ) ) ;
#4077 = VERTEX_POINT ( 'NONE', #979 ) ;
#4078 = AXIS2_PLACEMENT_3D ( 'NONE', #4505, #2668, #10193 ) ;
#4079 = VERTEX_POINT ( 'NONE', #9242 ) ;
#4080 = FACE_OUTER_BOUND ( 'NONE', #7329, .T. ) ;
#4081 = CARTESIAN_POINT ( 'NONE',  ( 3.000000000000000888, -21.14796121233190362, -9.039786367039052806 ) ) ;
#4082 = AXIS2_PLACEMENT_3D ( 'NONE', #3593, #4572, #6400 ) ;
#4083 = DIRECTION ( 'NONE',  ( -1.000000000000000000, 0.000000000000000000, -0.000000000000000000 ) ) ;
#4084 = FACE_OUTER_BOUND ( 'NONE', #471, .T. ) ;
#4085 = CIRCLE ( 'NONE', #5649, 9.599999999999996092 ) ;
#4086 = EDGE_CURVE ( 'NONE', #4836, #679, #9013, .T. ) ;
#4087 = CARTESIAN_POINT ( 'NONE',  ( 2.355103038863950893, 10.93470652055903791, 3.747395293195558847E-16 ) ) ;
#4088 = CARTESIAN_POINT ( 'NONE',  ( 0.000000000000000000, 0.000000000000000000, 0.000000000000000000 ) ) ;
#4089 = ORIENTED_EDGE ( 'NONE', *, *, #6921, .T. ) ;
#4090 = VERTEX_POINT ( 'NONE', #4596 ) ;
#4091 = APPLICATION_PROTOCOL_DEFINITION ( 'draft international standard', 'automotive_design', 1998, #7781 ) ;
#4092 = CARTESIAN_POINT ( 'NONE',  ( 7.525577113297165610, 13.03378399180780889, 10.00000000000000000 ) ) ;
#4093 = ORIENTED_EDGE ( 'NONE', *, *, #2993, .T. ) ;
#4094 = CYLINDRICAL_SURFACE ( 'NONE', #8385, 9.599999999999997868 ) ;
#4095 = CYLINDRICAL_SURFACE ( 'NONE', #4285, 9.599999999999997868 ) ;
#4096 = CARTESIAN_POINT ( 'NONE',  ( 1.500000000000000444, -23.24434456306330787, 8.645255683528924706 ) ) ;
#4097 = ORIENTED_EDGE ( 'NONE', *, *, #2550, .T. ) ;
#4098 = LINE ( 'NONE', #3067, #2213 ) ;
#4099 = AXIS2_PLACEMENT_3D ( 'NONE', #2997, #6832, #7700 ) ;
#4100 = DIRECTION ( 'NONE',  ( -1.000000000000000000, 0.000000000000000000, 0.000000000000000000 ) ) ;
#4101 = CARTESIAN_POINT ( 'NONE',  ( -11.98007164540816838, 10.17225797950327681, 6.857782953271941950E-17 ) ) ;
#4102 = EDGE_LOOP ( 'NONE', ( #648, #2307, #11940, #11990 ) ) ;
#4103 = DIRECTION ( 'NONE',  ( -1.000000000000000000, -0.000000000000000000, -0.000000000000000000 ) ) ;
#4104 = EDGE_LOOP ( 'NONE', ( #5234, #8691 ) ) ;
#4105 = CARTESIAN_POINT ( 'NONE',  ( 3.000000000000000888, 7.432877647175206270, 21.76479567747243848 ) ) ;
#4106 = AXIS2_PLACEMENT_3D ( 'NONE', #3524, #7236, #1559 ) ;
#4107 = ORIENTED_EDGE ( 'NONE', *, *, #3112, .T. ) ;
#4108 = EDGE_CURVE ( 'NONE', #8051, #1936, #1390, .T. ) ;
#4109 = CARTESIAN_POINT ( 'NONE',  ( 3.053028024665676021, -9.450988318042126579, 10.00000000000000000 ) ) ;
#4110 = AXIS2_PLACEMENT_3D ( 'NONE', #9511, #2227, #2105 ) ;
#4111 = CARTESIAN_POINT ( 'NONE',  ( 0.000000000000000000, 0.000000000000000000, 0.000000000000000000 ) ) ;
#4112 = SURFACE_SIDE_STYLE ('',( #2154 ) ) ;
#4113 = EDGE_CURVE ( 'NONE', #1752, #1491, #8235, .T. ) ;
#4114 = DIRECTION ( 'NONE',  ( -1.000000000000000000, 0.000000000000000000, 0.000000000000000000 ) ) ;
#4115 = DIRECTION ( 'NONE',  ( 0.000000000000000000, 0.4067366430758009299, -0.9135454576426005335 ) ) ;
#4116 = CARTESIAN_POINT ( 'NONE',  ( -7.159234172427928478, 10.34564589702411475, 10.00000000000000000 ) ) ;
#4117 = AXIS2_PLACEMENT_3D ( 'NONE', #7221, #687, #4359 ) ;
#4118 = DIRECTION ( 'NONE',  ( 0.000000000000000000, 0.000000000000000000, 1.000000000000000000 ) ) ;
#4119 = CIRCLE ( 'NONE', #7230, 22.99899999999999523 ) ;
#4120 = CARTESIAN_POINT ( 'NONE',  ( -9.470608727120474413, 11.15741021143934297, 3.747395293195558847E-16 ) ) ;
#4121 = AXIS2_PLACEMENT_3D ( 'NONE', #2770, #10106, #68 ) ;
#4122 = EDGE_CURVE ( 'NONE', #2635, #6096, #918, .T. ) ;
#4123 = DIRECTION ( 'NONE',  ( -0.000000000000000000, -0.000000000000000000, -1.000000000000000000 ) ) ;
#4124 = STYLED_ITEM ( 'NONE', ( #10717 ), #7312 ) ;
#4125 = LINE ( 'NONE', #8600, #11917 ) ;
#4126 = EDGE_CURVE ( 'NONE', #9529, #11898, #6087, .T. ) ;
#4127 = ORIENTED_EDGE ( 'NONE', *, *, #11043, .F. ) ;
#4128 = ORIENTED_EDGE ( 'NONE', *, *, #11678, .F. ) ;
#4129 = ORIENTED_EDGE ( 'NONE', *, *, #8084, .T. ) ;
#4130 = AXIS2_PLACEMENT_3D ( 'NONE', #1785, #2647, #6555 ) ;
#4131 = VECTOR ( 'NONE', #276, 1000.000000000000000 ) ;
#4132 = CARTESIAN_POINT ( 'NONE',  ( 3.000000000000000888, -24.02068490260617040, 6.168200451485680524 ) ) ;
#4133 = AXIS2_PLACEMENT_3D ( 'NONE', #2448, #4227, #6188 ) ;
#4134 = DIRECTION ( 'NONE',  ( 0.000000000000000000, 0.000000000000000000, 1.000000000000000000 ) ) ;
#4135 = DIRECTION ( 'NONE',  ( -1.000000000000000000, 0.000000000000000000, 0.000000000000000000 ) ) ;
#4136 = CARTESIAN_POINT ( 'NONE',  ( -4.625218816435448410, 8.325684435358759572, 10.00000000000000000 ) ) ;
#4137 = CARTESIAN_POINT ( 'NONE',  ( -6.864300873105353418, 13.92024697337931549, 6.857782953271941950E-17 ) ) ;
#4138 = DIRECTION ( 'NONE',  ( -1.000000000000000000, -0.000000000000000000, -0.000000000000000000 ) ) ;
#4139 = DIRECTION ( 'NONE',  ( -0.000000000000000000, -0.000000000000000000, -1.000000000000000000 ) ) ;
#4140 = CIRCLE ( 'NONE', #6861, 24.80000000000000071 ) ;
#4141 = ORIENTED_EDGE ( 'NONE', *, *, #3174, .T. ) ;
#4142 = AXIS2_PLACEMENT_3D ( 'NONE', #11100, #4558, #4619 ) ;
#4143 = VERTEX_POINT ( 'NONE', #7520 ) ;
#4144 = ORIENTED_EDGE ( 'NONE', *, *, #392, .T. ) ;
#4145 = FACE_OUTER_BOUND ( 'NONE', #11381, .T. ) ;
#4146 = AXIS2_PLACEMENT_3D ( 'NONE', #2646, #805, #3507 ) ;
#4147 = PRODUCT_DEFINITION_SHAPE ( 'NONE', 'NONE',  #12123 ) ;
#4148 = VECTOR ( 'NONE', #3987, 1000.000000000000000 ) ;
#4149 = FACE_BOUND ( 'NONE', #10153, .T. ) ;
#4150 = DIRECTION ( 'NONE',  ( 1.000000000000000000, -0.000000000000000000, 0.000000000000000000 ) ) ;
#4151 = CIRCLE ( 'NONE', #4335, 9.599999999999997868 ) ;
#4152 = DIRECTION ( 'NONE',  ( -1.000000000000000000, -0.000000000000000000, 0.000000000000000000 ) ) ;
#4153 = CARTESIAN_POINT ( 'NONE',  ( -3.937910939466568117, -8.732312745279397603, 3.747395293195558847E-16 ) ) ;
#4154 = EDGE_CURVE ( 'NONE', #10713, #5976, #11264, .T. ) ;
#4155 = CARTESIAN_POINT ( 'NONE',  ( 3.000000000000000888, 0.000000000000000000, 0.000000000000000000 ) ) ;
#4156 = ORIENTED_EDGE ( 'NONE', *, *, #368, .T. ) ;
#4157 = ORIENTED_EDGE ( 'NONE', *, *, #2355, .T. ) ;
#4158 = CARTESIAN_POINT ( 'NONE',  ( 4.479449988082535583, -13.21383449271838550, 10.00000000000000000 ) ) ;
#4159 = CIRCLE ( 'NONE', #10407, 1.500000000000000222 ) ;
#4160 = ORIENTED_EDGE ( 'NONE', *, *, #5987, .F. ) ;
#4161 = CYLINDRICAL_SURFACE ( 'NONE', #2516, 9.599999999999997868 ) ;
#4162 = LINE ( 'NONE', #5135, #2808 ) ;
#4163 = ADVANCED_FACE ( 'NONE', ( #11495 ), #3855, .T. ) ;
#4164 = CARTESIAN_POINT ( 'NONE',  ( 0.000000000000000000, 15.40502424595145037, 19.43515443678408516 ) ) ;
#4165 = VERTEX_POINT ( 'NONE', #5872 ) ;
#4166 = CIRCLE ( 'NONE', #3199, 22.99900000000000588 ) ;
#4167 = CARTESIAN_POINT ( 'NONE',  ( 3.000000000000000888, 0.000000000000000000, 0.000000000000000000 ) ) ;
#4168 = DIRECTION ( 'NONE',  ( 0.000000000000000000, 0.5000000000000011102, -0.8660254037844381525 ) ) ;
#4169 = CARTESIAN_POINT ( 'NONE',  ( -5.965338750500049692, 7.524205049158500636, 6.857782953271941950E-17 ) ) ;
#4170 = ORIENTED_EDGE ( 'NONE', *, *, #10915, .T. ) ;
#4171 = CARTESIAN_POINT ( 'NONE',  ( 3.000000000000000888, -24.45282072769598258, -4.135161237383832677 ) ) ;
#4172 = CYLINDRICAL_SURFACE ( 'NONE', #5889, 24.80000000000000071 ) ;
#4173 = VERTEX_POINT ( 'NONE', #11438 ) ;
#4174 = AXIS2_PLACEMENT_3D ( 'NONE', #3742, #7465, #174 ) ;
#4175 = CARTESIAN_POINT ( 'NONE',  ( -9.037587479195734019, -0.7561632655184234997, 10.00000000000000000 ) ) ;
#4176 = CIRCLE ( 'NONE', #10030, 22.99899999999999523 ) ;
#4177 = DIRECTION ( 'NONE',  ( -1.000000000000000000, 0.000000000000000000, -0.000000000000000000 ) ) ;
#4178 = ORIENTED_EDGE ( 'NONE', *, *, #10819, .F. ) ;
#4179 = FACE_OUTER_BOUND ( 'NONE', #11279, .T. ) ;
#4180 = DIRECTION ( 'NONE',  ( 0.000000000000000000, 0.1045284632676536929, -0.9945218953682732899 ) ) ;
#4181 = CARTESIAN_POINT ( 'NONE',  ( 5.835571643920557605, -9.386589068694828342, 10.00000000000000000 ) ) ;
#4182 = AXIS2_PLACEMENT_3D ( 'NONE', #5139, #1702, #3297 ) ;
#4183 = FILL_AREA_STYLE_COLOUR ( '', #11182 ) ;
#4184 = CARTESIAN_POINT ( 'NONE',  ( -1.036640877615904843, -15.73686152240404468, 3.747395293195558847E-16 ) ) ;
#4185 = FACE_OUTER_BOUND ( 'NONE', #5491, .T. ) ;
#4186 = VERTEX_POINT ( 'NONE', #10514 ) ;
#4187 = DIRECTION ( 'NONE',  ( -1.000000000000000000, -0.000000000000000000, 0.000000000000000000 ) ) ;
#4188 = ORIENTED_EDGE ( 'NONE', *, *, #9521, .T. ) ;
#4189 = EDGE_CURVE ( 'NONE', #5168, #4720, #6600, .T. ) ;
#4190 = FACE_OUTER_BOUND ( 'NONE', #7330, .T. ) ;
#4191 = DIRECTION ( 'NONE',  ( 0.000000000000000000, 0.000000000000000000, 1.000000000000000000 ) ) ;
#4192 = EDGE_CURVE ( 'NONE', #5574, #5856, #7849, .T. ) ;
#4193 = CARTESIAN_POINT ( 'NONE',  ( 0.000000000000000000, -1.556492618230806535, 24.75110766671651774 ) ) ;
#4194 = CARTESIAN_POINT ( 'NONE',  ( 6.396238541183701720, 6.183590428399974748, 10.00000000000000000 ) ) ;
#4195 = CARTESIAN_POINT ( 'NONE',  ( 5.027256439335598515, -9.798587832408038878, 6.857782953271941950E-17 ) ) ;
#4196 = FILL_AREA_STYLE_COLOUR ( '', #5502 ) ;
#4197 = EDGE_CURVE ( 'NONE', #6189, #11027, #8636, .T. ) ;
#4198 = CIRCLE ( 'NONE', #12003, 22.99899999999999523 ) ;
#4199 = CARTESIAN_POINT ( 'NONE',  ( 3.000000000000000888, 22.37663021667344054, 6.788022064062137595 ) ) ;
#4200 = ORIENTED_EDGE ( 'NONE', *, *, #5714, .F. ) ;
#4201 = ORIENTED_EDGE ( 'NONE', *, *, #2172, .F. ) ;
#4202 = VERTEX_POINT ( 'NONE', #5694 ) ;
#4203 = DIRECTION ( 'NONE',  ( 0.000000000000000000, -0.4067366430758072582, 0.9135454576425977580 ) ) ;
#4204 = DIRECTION ( 'NONE',  ( -1.000000000000000000, 0.000000000000000000, 0.000000000000000000 ) ) ;
#4205 = CARTESIAN_POINT ( 'NONE',  ( 0.000000000000000000, -20.78471918669866270, 8.753070780933086326 ) ) ;
#4206 = CARTESIAN_POINT ( 'NONE',  ( -10.73274959028096198, -5.974010873319483217, 3.747395293195558847E-16 ) ) ;
#4207 = CARTESIAN_POINT ( 'NONE',  ( 3.000000000000000888, -20.86861857134741172, 9.667200211209745930 ) ) ;
#4208 = DIRECTION ( 'NONE',  ( -1.000000000000000000, -0.000000000000000000, 0.000000000000000000 ) ) ;
#4209 = EDGE_LOOP ( 'NONE', ( #7969, #2500 ) ) ;
#4210 = ORIENTED_EDGE ( 'NONE', *, *, #10659, .T. ) ;
#4211 = EDGE_CURVE ( 'NONE', #5043, #1562, #4537, .T. ) ;
#4212 = CARTESIAN_POINT ( 'NONE',  ( -7.159234172427928478, 10.34564589702411475, 10.00000000000000000 ) ) ;
#4213 = ORIENTED_EDGE ( 'NONE', *, *, #3677, .T. ) ;
#4214 = DIRECTION ( 'NONE',  ( -1.000000000000000000, 0.000000000000000000, 0.000000000000000000 ) ) ;
#4215 = FACE_BOUND ( 'NONE', #10718, .T. ) ;
#4216 = EDGE_CURVE ( 'NONE', #9404, #1587, #8447, .T. ) ;
#4217 = DIRECTION ( 'NONE',  ( 0.000000000000000000, 1.000000000000000000, 3.491481338843133355E-15 ) ) ;
#4218 = ORIENTED_EDGE ( 'NONE', *, *, #1943, .F. ) ;
#4219 = CARTESIAN_POINT ( 'NONE',  ( 0.000000000000000000, 20.08719549084880640, -11.20082935824054182 ) ) ;
#4220 = AXIS2_PLACEMENT_3D ( 'NONE', #1533, #11996, #7093 ) ;
#4221 = DIRECTION ( 'NONE',  ( 0.000000000000000000, 0.000000000000000000, 1.000000000000000000 ) ) ;
#4222 = CARTESIAN_POINT ( 'NONE',  ( 8.025946968469181542, -7.769110617520081696, 6.857782953271941950E-17 ) ) ;
#4223 = ORIENTED_EDGE ( 'NONE', *, *, #7185, .T. ) ;
#4224 = EDGE_CURVE ( 'NONE', #5646, #6550, #3333, .T. ) ;
#4225 = CARTESIAN_POINT ( 'NONE',  ( 1.499999999999999556, -11.48910920600668284, -21.97817939804051690 ) ) ;
#4226 = VERTEX_POINT ( 'NONE', #5228 ) ;
#4227 = DIRECTION ( 'NONE',  ( -1.000000000000000000, 0.000000000000000000, 0.000000000000000000 ) ) ;
#4228 = ORIENTED_EDGE ( 'NONE', *, *, #2268, .F. ) ;
#4229 = CARTESIAN_POINT ( 'NONE',  ( 8.282588618526579793, 7.043362411858248073, 10.00000000000000000 ) ) ;
#4230 = ORIENTED_EDGE ( 'NONE', *, *, #8102, .T. ) ;
#4231 = DIRECTION ( 'NONE',  ( 0.000000000000000000, 0.000000000000000000, -1.000000000000000000 ) ) ;
#4232 = DIRECTION ( 'NONE',  ( -1.000000000000000000, 0.000000000000000000, 0.000000000000000000 ) ) ;
#4233 = ORIENTED_EDGE ( 'NONE', *, *, #4814, .T. ) ;
#4234 = DIRECTION ( 'NONE',  ( 0.000000000000000000, 0.000000000000000000, 1.000000000000000000 ) ) ;
#4235 = DIRECTION ( 'NONE',  ( -1.000000000000000000, -0.000000000000000000, 0.000000000000000000 ) ) ;
#4236 = CARTESIAN_POINT ( 'NONE',  ( 8.393308867179015920, -1.106660293010312657, 10.00000000000000000 ) ) ;
#4237 = EDGE_CURVE ( 'NONE', #3881, #1864, #8961, .T. ) ;
#4238 = CARTESIAN_POINT ( 'NONE',  ( 0.000000000000000000, -15.80756504416703656, 19.10918332567953115 ) ) ;
#4239 = CARTESIAN_POINT ( 'NONE',  ( 12.15471013770256903, -5.500887282572993975, 3.747395293195558847E-16 ) ) ;
#4240 = FACE_OUTER_BOUND ( 'NONE', #1280, .T. ) ;
#4241 = DIRECTION ( 'NONE',  ( 0.000000000000000000, 0.000000000000000000, 1.000000000000000000 ) ) ;
#4242 = VERTEX_POINT ( 'NONE', #7113 ) ;
#4243 = CYLINDRICAL_SURFACE ( 'NONE', #2849, 9.599999999999997868 ) ;
#4244 = ORIENTED_EDGE ( 'NONE', *, *, #2275, .T. ) ;
#4245 = DIRECTION ( 'NONE',  ( 1.000000000000000000, 0.000000000000000000, 0.000000000000000000 ) ) ;
#4246 = CYLINDRICAL_SURFACE ( 'NONE', #1780, 9.599999999999997868 ) ;
#4247 = DIRECTION ( 'NONE',  ( -0.000000000000000000, -0.000000000000000000, 1.000000000000000000 ) ) ;
#4248 = CARTESIAN_POINT ( 'NONE',  ( -3.542987847618590536, 5.503081486278161627, 10.00000000000000000 ) ) ;
#4249 = CARTESIAN_POINT ( 'NONE',  ( -1.672018190274121574, 9.216430685901386255, 6.857782953271941950E-17 ) ) ;
#4250 = DIRECTION ( 'NONE',  ( -1.000000000000000000, 0.000000000000000000, -0.000000000000000000 ) ) ;
#4251 = LINE ( 'NONE', #1441, #2940 ) ;
#4252 = ORIENTED_EDGE ( 'NONE', *, *, #8693, .F. ) ;
#4253 = AXIS2_PLACEMENT_3D ( 'NONE', #6071, #7907, #1357 ) ;
#4254 = VERTEX_POINT ( 'NONE', #10865 ) ;
#4255 = EDGE_CURVE ( 'NONE', #2419, #6911, #2476, .T. ) ;
#4256 = VERTEX_POINT ( 'NONE', #10358 ) ;
#4257 = CARTESIAN_POINT ( 'NONE',  ( -13.83044629298881389, 5.462350471645223138, 10.00000000000000000 ) ) ;
#4258 = EDGE_CURVE ( 'NONE', #4254, #10458, #614, .T. ) ;
#4259 = CARTESIAN_POINT ( 'NONE',  ( 1.500000000000000222, 0.000000000000000000, -15.00000000000000000 ) ) ;
#4260 = CARTESIAN_POINT ( 'NONE',  ( -22.00000000000000000, 0.000000000000000000, 20.00000000000000000 ) ) ;
#4261 = CARTESIAN_POINT ( 'NONE',  ( 5.498207398720008854, -4.630339417915828371, 3.747395293195558847E-16 ) ) ;
#4262 = LINE ( 'NONE', #4389, #3154 ) ;
#4263 = EDGE_CURVE ( 'NONE', #8927, #4549, #9414, .T. ) ;
#4264 = CARTESIAN_POINT ( 'NONE',  ( 0.000000000000000000, 0.000000000000000000, 0.000000000000000000 ) ) ;
#4265 = EDGE_LOOP ( 'NONE', ( #7460, #6887, #3853, #10777 ) ) ;
#4266 = EDGE_LOOP ( 'NONE', ( #11277, #534, #7070, #8913 ) ) ;
#4267 = SHAPE_DEFINITION_REPRESENTATION ( #3171, #6698 ) ;
#4268 = CARTESIAN_POINT ( 'NONE',  ( 8.588976300537440878, -11.19439025337201343, 10.00000000000000000 ) ) ;
#4269 = EDGE_CURVE ( 'NONE', #5364, #3541, #4534, .T. ) ;
#4270 = VERTEX_POINT ( 'NONE', #9326 ) ;
#4271 = CARTESIAN_POINT ( 'NONE',  ( -3.038216613430223756, 4.635879136410493651, 10.00000000000000000 ) ) ;
#4272 = AXIS2_PLACEMENT_3D ( 'NONE', #1134, #3835, #4869 ) ;
#4273 = FACE_OUTER_BOUND ( 'NONE', #10488, .T. ) ;
#4274 = DIRECTION ( 'NONE',  ( -1.000000000000000000, -0.000000000000000000, 0.000000000000000000 ) ) ;
#4275 = FACE_OUTER_BOUND ( 'NONE', #398, .T. ) ;
#4276 = ORIENTED_EDGE ( 'NONE', *, *, #3448, .T. ) ;
#4277 = CARTESIAN_POINT ( 'NONE',  ( 0.000000000000000000, -6.668524164681463695, -23.88662356770121775 ) ) ;
#4278 = DIRECTION ( 'NONE',  ( -1.000000000000000000, 0.000000000000000000, 0.000000000000000000 ) ) ;
#4279 = CARTESIAN_POINT ( 'NONE',  ( -1.410059164928062048, 12.26527237696109474, 6.857782953271941950E-17 ) ) ;
#4280 = CIRCLE ( 'NONE', #2527, 22.99900000000000233 ) ;
#4281 = CARTESIAN_POINT ( 'NONE',  ( 0.000000000000000000, 0.000000000000000000, 0.000000000000000000 ) ) ;
#4282 = LINE ( 'NONE', #10712, #2965 ) ;
#4283 = ORIENTED_EDGE ( 'NONE', *, *, #9289, .T. ) ;
#4284 = CARTESIAN_POINT ( 'NONE',  ( -10.73274959028002229, -5.974010873319484105, 10.00000000000000000 ) ) ;
#4285 = AXIS2_PLACEMENT_3D ( 'NONE', #7825, #8874, #6051 ) ;
#4286 = AXIS2_PLACEMENT_3D ( 'NONE', #4704, #2930, #1037 ) ;
#4287 = LINE ( 'NONE', #10782, #12033 ) ;
#4288 = CARTESIAN_POINT ( 'NONE',  ( 1.500000000000000444, -1.039229259764318680, -24.77821629063823394 ) ) ;
#4289 = CIRCLE ( 'NONE', #1366, 9.599999999999999645 ) ;
#4290 = CARTESIAN_POINT ( 'NONE',  ( 3.000000000000000888, -6.532525787310825116, -21.58580335785683246 ) ) ;
#4291 = CARTESIAN_POINT ( 'NONE',  ( 1.500000000000000444, 23.24434456306337182, -8.645255683528766610 ) ) ;
#4292 = CARTESIAN_POINT ( 'NONE',  ( -9.386162357322616501, -4.067606288967439809, 10.00000000000000000 ) ) ;
#4293 = DIRECTION ( 'NONE',  ( 0.000000000000000000, 0.000000000000000000, 1.000000000000000000 ) ) ;
#4294 = CARTESIAN_POINT ( 'NONE',  ( 10.44364468045615801, 9.157203537817473205, 3.747395293195558847E-16 ) ) ;
#4295 = ADVANCED_FACE ( 'NONE', ( #821 ), #8290, .T. ) ;
#4296 = DIRECTION ( 'NONE',  ( 0.000000000000000000, 0.000000000000000000, 1.000000000000000000 ) ) ;
#4297 = ORIENTED_EDGE ( 'NONE', *, *, #10763, .T. ) ;
#4298 = DIRECTION ( 'NONE',  ( 0.000000000000000000, 0.000000000000000000, 1.000000000000000000 ) ) ;
#4299 = VERTEX_POINT ( 'NONE', #12016 ) ;
#4300 = DIRECTION ( 'NONE',  ( -1.000000000000000000, -0.000000000000000000, 0.000000000000000000 ) ) ;
#4301 = CARTESIAN_POINT ( 'NONE',  ( 3.000000000000000888, -19.74380051311548456, 11.79560690673865331 ) ) ;
#4302 = ORIENTED_EDGE ( 'NONE', *, *, #11233, .F. ) ;
#4303 = ADVANCED_FACE ( 'NONE', ( #12071 ), #2717, .T. ) ;
#4304 = CIRCLE ( 'NONE', #11150, 18.49999999999999645 ) ;
#4305 = FACE_OUTER_BOUND ( 'NONE', #7639, .T. ) ;
#4306 = VECTOR ( 'NONE', #5027, 1000.000000000000000 ) ;
#4307 = CYLINDRICAL_SURFACE ( 'NONE', #2030, 9.599999999999997868 ) ;
#4308 = DIRECTION ( 'NONE',  ( 0.000000000000000000, -0.2079116908177468526, -0.9781476007338083534 ) ) ;
#4309 = CARTESIAN_POINT ( 'NONE',  ( 10.90031251054715966, 4.301772984117409493, 6.857782953271941950E-17 ) ) ;
#4310 = CYLINDRICAL_SURFACE ( 'NONE', #8067, 22.99899999999999878 ) ;
#4311 = LINE ( 'NONE', #11780, #9384 ) ;
#4312 = ORIENTED_EDGE ( 'NONE', *, *, #4792, .F. ) ;
#4313 = AXIS2_PLACEMENT_3D ( 'NONE', #6851, #4908, #7719 ) ;
#4314 = ORIENTED_EDGE ( 'NONE', *, *, #256, .T. ) ;
#4315 = AXIS2_PLACEMENT_3D ( 'NONE', #11864, #4347, #10954 ) ;
#4316 = ORIENTED_EDGE ( 'NONE', *, *, #6137, .T. ) ;
#4317 = AXIS2_PLACEMENT_3D ( 'NONE', #4703, #9291, #2809 ) ;
#4318 = PRODUCT_DEFINITION_FORMATION_WITH_SPECIFIED_SOURCE ( 'ANY', '', #6001, .NOT_KNOWN. ) ;
#4319 = CARTESIAN_POINT ( 'NONE',  ( 4.977139221860650942, 13.21892491369670530, 10.00000000000000000 ) ) ;
#4320 = SURFACE_SIDE_STYLE ('',( #5182 ) ) ;
#4321 = DIRECTION ( 'NONE',  ( 0.000000000000000000, 0.000000000000000000, -1.000000000000000000 ) ) ;
#4322 = AXIS2_PLACEMENT_3D ( 'NONE', #1055, #7003, #4784 ) ;
#4323 = CIRCLE ( 'NONE', #1018, 9.599999999999996092 ) ;
#4324 = CARTESIAN_POINT ( 'NONE',  ( 3.656769781543557141, 7.172433557890304456, 3.747395293195558847E-16 ) ) ;
#4325 = DIRECTION ( 'NONE',  ( 0.000000000000000000, 0.000000000000000000, 1.000000000000000000 ) ) ;
#4326 = LINE ( 'NONE', #3285, #5272 ) ;
#4327 = ORIENTED_EDGE ( 'NONE', *, *, #7498, .F. ) ;
#4328 = ORIENTED_EDGE ( 'NONE', *, *, #7237, .F. ) ;
#4329 = AXIS2_PLACEMENT_3D ( 'NONE', #9809, #4357, #2400 ) ;
#4330 = ORIENTED_EDGE ( 'NONE', *, *, #10248, .F. ) ;
#4331 = CARTESIAN_POINT ( 'NONE',  ( 3.678979105947490780, -2.215585777442456550, 10.00000000000000000 ) ) ;
#4332 = ADVANCED_FACE ( 'NONE', ( #11167 ), #10310, .F. ) ;
#4333 = DIRECTION ( 'NONE',  ( 0.000000000000000000, 0.000000000000000000, -1.000000000000000000 ) ) ;
#4334 = DIRECTION ( 'NONE',  ( 0.000000000000000000, 0.7431448254773909134, 0.6691306063588620123 ) ) ;
#4335 = AXIS2_PLACEMENT_3D ( 'NONE', #3193, #9912, #6127 ) ;
#4336 = CYLINDRICAL_SURFACE ( 'NONE', #5412, 9.599999999999997868 ) ;
#4337 = VERTEX_POINT ( 'NONE', #1704 ) ;
#4338 = PRODUCT_RELATED_PRODUCT_CATEGORY ( 'part', '', ( #11573 ) ) ;
#4339 = DIRECTION ( 'NONE',  ( -1.000000000000000000, 0.000000000000000000, 0.000000000000000000 ) ) ;
#4340 = EDGE_CURVE ( 'NONE', #1307, #5268, #10776, .T. ) ;
#4341 = LINE ( 'NONE', #5436, #1409 ) ;
#4342 = CARTESIAN_POINT ( 'NONE',  ( -2.433178163897522506, 9.086443520544598584, 6.857782953271941950E-17 ) ) ;
#4343 = CIRCLE ( 'NONE', #2190, 22.99900000000000233 ) ;
#4344 = CIRCLE ( 'NONE', #11581, 24.80000000000000071 ) ;
#4345 = EDGE_CURVE ( 'NONE', #6529, #7759, #4528, .T. ) ;
#4346 = LINE ( 'NONE', #11630, #7828 ) ;
#4347 = DIRECTION ( 'NONE',  ( -1.000000000000000000, 0.000000000000000000, 0.000000000000000000 ) ) ;
#4348 = EDGE_LOOP ( 'NONE', ( #10105, #7581, #5410, #3251 ) ) ;
#4349 = CARTESIAN_POINT ( 'NONE',  ( 4.212679447664378074, 6.814025269448781508, 10.00000000000000000 ) ) ;
#4350 = CIRCLE ( 'NONE', #7672, 22.00000000000000000 ) ;
#4351 = ORIENTED_EDGE ( 'NONE', *, *, #2420, .T. ) ;
#4352 = DIRECTION ( 'NONE',  ( -1.000000000000000000, -0.000000000000000000, -0.000000000000000000 ) ) ;
#4353 = VERTEX_POINT ( 'NONE', #9237 ) ;
#4354 = FACE_OUTER_BOUND ( 'NONE', #9944, .T. ) ;
#4355 = DIRECTION ( 'NONE',  ( 0.000000000000000000, 1.000000000000000000, 3.614007241618349165E-15 ) ) ;
#4356 = CARTESIAN_POINT ( 'NONE',  ( 9.774996403550735735, -5.644905071530105900, 10.00000000000000000 ) ) ;
#4357 = DIRECTION ( 'NONE',  ( 1.000000000000000000, 0.000000000000000000, 0.000000000000000000 ) ) ;
#4358 = CARTESIAN_POINT ( 'NONE',  ( -4.054747718262373901, -11.96785467447665674, 3.747395293195558847E-16 ) ) ;
#4359 = DIRECTION ( 'NONE',  ( 0.000000000000000000, 0.4067366430758009299, -0.9135454576426005335 ) ) ;
#4360 = AXIS2_PLACEMENT_3D ( 'NONE', #11569, #2083, #1163 ) ;
#4361 = ORIENTED_EDGE ( 'NONE', *, *, #669, .F. ) ;
#4362 = FACE_OUTER_BOUND ( 'NONE', #7993, .T. ) ;
#4363 = ORIENTED_EDGE ( 'NONE', *, *, #4977, .F. ) ;
#4364 = AXIS2_PLACEMENT_3D ( 'NONE', #11564, #1335, #9607 ) ;
#4365 = DIRECTION ( 'NONE',  ( 0.000000000000000000, 0.000000000000000000, -1.000000000000000000 ) ) ;
#4366 = CARTESIAN_POINT ( 'NONE',  ( 0.000000000000000000, 20.41249101028211754, -9.589108953447965433 ) ) ;
#4367 = SURFACE_SIDE_STYLE ('',( #11042 ) ) ;
#4368 = ORIENTED_EDGE ( 'NONE', *, *, #3665, .F. ) ;
#4369 = EDGE_CURVE ( 'NONE', #10077, #7105, #11071, .T. ) ;
#4370 = AXIS2_PLACEMENT_3D ( 'NONE', #1650, #5384, #9111 ) ;
#4371 = CARTESIAN_POINT ( 'NONE',  ( 0.000000000000000000, 0.000000000000000000, -15.00000000000000000 ) ) ;
#4372 = FACE_OUTER_BOUND ( 'NONE', #7214, .T. ) ;
#4373 = DIRECTION ( 'NONE',  ( 1.000000000000000000, 0.000000000000000000, 0.000000000000000000 ) ) ;
#4374 = CARTESIAN_POINT ( 'NONE',  ( -6.451445390047177320, -3.308750875808899483, 10.00000000000000000 ) ) ;
#4375 = MANIFOLD_SOLID_BREP ( 'Boss-Extrude2', #11367 ) ;
#4376 = CARTESIAN_POINT ( 'NONE',  ( -1.916691774771271284, -10.52688368019216014, 6.857782953271941950E-17 ) ) ;
#4377 = DIRECTION ( 'NONE',  ( -6.938893903907228378E-16, -0.000000000000000000, -1.000000000000000000 ) ) ;
#4378 = LINE ( 'NONE', #4199, #3165 ) ;
#4379 = ORIENTED_EDGE ( 'NONE', *, *, #851, .F. ) ;
#4380 = ADVANCED_FACE ( 'NONE', ( #6818 ), #274, .T. ) ;
#4381 = ORIENTED_EDGE ( 'NONE', *, *, #11063, .F. ) ;
#4382 = AXIS2_PLACEMENT_3D ( 'NONE', #6155, #159, #2069 ) ;
#4383 = ORIENTED_EDGE ( 'NONE', *, *, #3300, .T. ) ;
#4384 = CARTESIAN_POINT ( 'NONE',  ( 9.683839015878914935, 10.01260560230626595, 10.00000000000000000 ) ) ;
#4385 = DIRECTION ( 'NONE',  ( 0.000000000000000000, 0.000000000000000000, -1.000000000000000000 ) ) ;
#4386 = CARTESIAN_POINT ( 'NONE',  ( 3.000000000000000888, 0.000000000000000000, 0.000000000000000000 ) ) ;
#4387 = AXIS2_PLACEMENT_3D ( 'NONE', #8091, #8276, #2457 ) ;
#4388 = CARTESIAN_POINT ( 'NONE',  ( -4.428608208598374674, -4.627450663480007442, 3.747395293195558847E-16 ) ) ;
#4389 = CARTESIAN_POINT ( 'NONE',  ( 1.500000000000000444, 20.65684170206509762, -13.72351598154876129 ) ) ;
#4390 = DIRECTION ( 'NONE',  ( -0.000000000000000000, -0.000000000000000000, -1.000000000000000000 ) ) ;
#4391 = ORIENTED_EDGE ( 'NONE', *, *, #9025, .F. ) ;
#4392 = VERTEX_POINT ( 'NONE', #5973 ) ;
#4393 = PRODUCT_CONTEXT ( 'NONE', #9663, 'mechanical' ) ;
#4394 = ORIENTED_EDGE ( 'NONE', *, *, #11265, .F. ) ;
#4395 = CARTESIAN_POINT ( 'NONE',  ( 0.000000000000000000, -22.21333432029556221, -11.02759168516767474 ) ) ;
#4396 = CYLINDRICAL_SURFACE ( 'NONE', #5858, 24.80000000000000071 ) ;
#4397 = CYLINDRICAL_SURFACE ( 'NONE', #3681, 22.99899999999999878 ) ;
#4398 = EDGE_LOOP ( 'NONE', ( #4363, #10890, #11810, #11623 ) ) ;
#4399 = DIRECTION ( 'NONE',  ( -1.000000000000000000, 0.000000000000000000, 0.000000000000000000 ) ) ;
#4400 = DIRECTION ( 'NONE',  ( 0.000000000000000000, 0.000000000000000000, 1.000000000000000000 ) ) ;
#4401 = CARTESIAN_POINT ( 'NONE',  ( 6.396238541184324333, 6.183590428399971195, 6.857782953271941950E-17 ) ) ;
#4402 = VECTOR ( 'NONE', #3458, 1000.000000000000000 ) ;
#4403 = DIRECTION ( 'NONE',  ( -1.000000000000000000, -0.000000000000000000, -0.000000000000000000 ) ) ;
#4404 = VERTEX_POINT ( 'NONE', #11259 ) ;
#4405 = CYLINDRICAL_SURFACE ( 'NONE', #1774, 9.599999999999999645 ) ;
#4406 = ORIENTED_EDGE ( 'NONE', *, *, #1797, .F. ) ;
#4407 = ORIENTED_EDGE ( 'NONE', *, *, #4636, .T. ) ;
#4408 = CARTESIAN_POINT ( 'NONE',  ( -1.784247137544766604, 5.123456263349899231, 10.00000000000000000 ) ) ;
#4409 = EDGE_CURVE ( 'NONE', #1752, #8897, #3747, .T. ) ;
#4410 = VERTEX_POINT ( 'NONE', #5050 ) ;
#4411 = LINE ( 'NONE', #8145, #5595 ) ;
#4412 = AXIS2_PLACEMENT_3D ( 'NONE', #6373, #5269, #11081 ) ;
#4413 = VERTEX_POINT ( 'NONE', #2873 ) ;
#4414 = EDGE_CURVE ( 'NONE', #12055, #4735, #2366, .T. ) ;
#4415 = DIRECTION ( 'NONE',  ( 1.000000000000000000, 0.000000000000000000, 0.000000000000000000 ) ) ;
#4416 = CARTESIAN_POINT ( 'NONE',  ( 0.000000000000000000, -22.90635393027947941, 2.062268319295487817 ) ) ;
#4417 = CARTESIAN_POINT ( 'NONE',  ( -7.130211940009574256, -7.605417807865423541, 10.00000000000000000 ) ) ;
#4418 = CARTESIAN_POINT ( 'NONE',  ( 0.000000000000000000, 0.000000000000000000, 0.000000000000000000 ) ) ;
#4419 = EDGE_LOOP ( 'NONE', ( #6632, #1029, #51, #716 ) ) ;
#4420 = AXIS2_PLACEMENT_3D ( 'NONE', #8829, #4177, #6972 ) ;
#4421 = ORIENTED_EDGE ( 'NONE', *, *, #6981, .T. ) ;
#4422 = CYLINDRICAL_SURFACE ( 'NONE', #1753, 9.599999999999997868 ) ;
#4423 = ORIENTED_EDGE ( 'NONE', *, *, #6179, .T. ) ;
#4424 = EDGE_CURVE ( 'NONE', #2739, #8206, #6289, .T. ) ;
#4425 = CARTESIAN_POINT ( 'NONE',  ( -6.012500708481076650, 0.06204199954272016787, 3.747395293195558847E-16 ) ) ;
#4426 = CARTESIAN_POINT ( 'NONE',  ( 3.000000000000000888, 0.000000000000000000, 0.000000000000000000 ) ) ;
#4427 = SHAPE_REPRESENTATION_RELATIONSHIP ( 'NONE' , 'NONE' ,  #5127, #6320 ) ;
#4428 = ORIENTED_EDGE ( 'NONE', *, *, #3022, .F. ) ;
#4429 = DIRECTION ( 'NONE',  ( 0.000000000000000000, 0.000000000000000000, 1.000000000000000000 ) ) ;
#4430 = AXIS2_PLACEMENT_3D ( 'NONE', #6488, #7462, #7525 ) ;
#4431 = DIRECTION ( 'NONE',  ( 0.000000000000000000, 0.000000000000000000, -1.000000000000000000 ) ) ;
#4432 = CARTESIAN_POINT ( 'NONE',  ( -2.682496113117368797, -7.114254743909099510, 10.00000000000000000 ) ) ;
#4433 = ADVANCED_FACE ( 'NONE', ( #3218 ), #4995, .T. ) ;
#4434 = CARTESIAN_POINT ( 'NONE',  ( -1.410059164928062048, 12.26527237696109474, 6.857782953271941950E-17 ) ) ;
#4435 = DIRECTION ( 'NONE',  ( -1.000000000000000000, -0.000000000000000000, 0.000000000000000000 ) ) ;
#4436 = DIRECTION ( 'NONE',  ( 0.000000000000000000, 0.000000000000000000, 1.000000000000000000 ) ) ;
#4437 = EDGE_LOOP ( 'NONE', ( #6068, #11579, #9747, #1434 ) ) ;
#4438 = EDGE_CURVE ( 'NONE', #5418, #9035, #2293, .T. ) ;
#4439 = EDGE_LOOP ( 'NONE', ( #4391, #6018, #5857, #2953 ) ) ;
#4440 = CARTESIAN_POINT ( 'NONE',  ( -9.470608727121586412, 11.15741021143934653, 10.00000000000000000 ) ) ;
#4441 = DIRECTION ( 'NONE',  ( -1.000000000000000000, 0.000000000000000000, 0.000000000000000000 ) ) ;
#4442 = DIRECTION ( 'NONE',  ( -1.000000000000000000, -0.000000000000000000, -0.000000000000000000 ) ) ;
#4443 = EDGE_CURVE ( 'NONE', #5009, #4610, #7742, .T. ) ;
#4444 = CARTESIAN_POINT ( 'NONE',  ( 6.841929108544086091, -2.672872603904024480, 3.747395293195558847E-16 ) ) ;
#4445 = AXIS2_PLACEMENT_3D ( 'NONE', #2531, #754, #6388 ) ;
#4446 = CARTESIAN_POINT ( 'NONE',  ( 0.000000000000000000, 22.99643626497956816, 0.3433949777332492848 ) ) ;
#4447 = EDGE_LOOP ( 'NONE', ( #11237, #5545, #8370, #1894 ) ) ;
#4448 = FACE_OUTER_BOUND ( 'NONE', #3654, .T. ) ;
#4449 = ADVANCED_FACE ( 'NONE', ( #7923 ), #3271, .T. ) ;
#4450 = ORIENTED_EDGE ( 'NONE', *, *, #10688, .T. ) ;
#4451 = SHAPE_DEFINITION_REPRESENTATION ( #325, #842 ) ;
#4452 = ORIENTED_EDGE ( 'NONE', *, *, #8969, .F. ) ;
#4453 = CARTESIAN_POINT ( 'NONE',  ( -4.158472309566741743, 3.840014155104743754, 10.00000000000000000 ) ) ;
#4454 = DIRECTION ( 'NONE',  ( 0.000000000000000000, 0.000000000000000000, 1.000000000000000000 ) ) ;
#4455 = CIRCLE ( 'NONE', #538, 24.80000000000000071 ) ;
#4456 = CARTESIAN_POINT ( 'NONE',  ( 0.000000000000000000, 0.000000000000000000, -15.00000000000000000 ) ) ;
#4457 = ADVANCED_FACE ( 'NONE', ( #6936 ), #6093, .T. ) ;
#4458 = CARTESIAN_POINT ( 'NONE',  ( 3.000000000000000888, 0.000000000000000000, 0.000000000000000000 ) ) ;
#4459 = CARTESIAN_POINT ( 'NONE',  ( 0.000000000000000000, -21.76479567747246691, 7.432877647175128999 ) ) ;
#4460 = CARTESIAN_POINT ( 'NONE',  ( -4.006926059188537614, 5.225193401749451461, 6.857782953271941950E-17 ) ) ;
#4461 = DIRECTION ( 'NONE',  ( 0.000000000000000000, 0.000000000000000000, -1.000000000000000000 ) ) ;
#4462 = CIRCLE ( 'NONE', #555, 24.80000000000000071 ) ;
#4463 = CARTESIAN_POINT ( 'NONE',  ( 0.000000000000000000, 10.87771529938162196, 19.75591328264889768 ) ) ;
#4464 = VERTEX_POINT ( 'NONE', #10557 ) ;
#4465 = ORIENTED_EDGE ( 'NONE', *, *, #510, .F. ) ;
#4466 = CARTESIAN_POINT ( 'NONE',  ( 5.498207398719435091, -4.630339417915830147, 10.00000000000000000 ) ) ;
#4467 = VERTEX_POINT ( 'NONE', #6883 ) ;
#4468 = CARTESIAN_POINT ( 'NONE',  ( 1.500000000000000444, -8.645255683528844770, -23.24434456306333985 ) ) ;
#4469 = ORIENTED_EDGE ( 'NONE', *, *, #214, .T. ) ;
#4470 = CIRCLE ( 'NONE', #5845, 9.599999999999996092 ) ;
#4471 = DIRECTION ( 'NONE',  ( 0.000000000000000000, -0.7431448254773862505, -0.6691306063588672304 ) ) ;
#4472 = CIRCLE ( 'NONE', #3111, 3.000000000000000444 ) ;
#4473 = CARTESIAN_POINT ( 'NONE',  ( 3.000000000000000888, 0.000000000000000000, 0.000000000000000000 ) ) ;
#4474 = CARTESIAN_POINT ( 'NONE',  ( -4.006926059189011902, 5.225193401749456790, 10.00000000000000000 ) ) ;
#4475 = LINE ( 'NONE', #11032, #9038 ) ;
#4476 = CARTESIAN_POINT ( 'NONE',  ( -3.000000000000000000, 3.673940397442059868E-16, -15.00000000000000000 ) ) ;
#4477 = ORIENTED_EDGE ( 'NONE', *, *, #7960, .T. ) ;
#4478 = EDGE_CURVE ( 'NONE', #5773, #6788, #4323, .T. ) ;
#4479 = DIRECTION ( 'NONE',  ( -1.000000000000000000, 0.000000000000000000, 0.000000000000000000 ) ) ;
#4480 = EDGE_LOOP ( 'NONE', ( #3392, #239, #2921, #6217 ) ) ;
#4481 = CIRCLE ( 'NONE', #8403, 24.80000000000000071 ) ;
#4482 = CIRCLE ( 'NONE', #11903, 24.80000000000000071 ) ;
#4483 = CARTESIAN_POINT ( 'NONE',  ( 4.340769014460001962, -0.9713985772308075806, 3.747395293195558847E-16 ) ) ;
#4484 = CIRCLE ( 'NONE', #2538, 22.99900000000000233 ) ;
#4485 = EDGE_CURVE ( 'NONE', #11794, #9479, #10920, .T. ) ;
#4486 = DIRECTION ( 'NONE',  ( -1.000000000000000000, -0.000000000000000000, 0.000000000000000000 ) ) ;
#4487 = PRESENTATION_STYLE_ASSIGNMENT (( #7109 ) ) ;
#4488 = ORIENTED_EDGE ( 'NONE', *, *, #11415, .F. ) ;
#4489 = CARTESIAN_POINT ( 'NONE',  ( 3.000000000000000888, 0.000000000000000000, 0.000000000000000000 ) ) ;
#4490 = DIRECTION ( 'NONE',  ( 0.000000000000000000, 0.000000000000000000, 1.000000000000000000 ) ) ;
#4491 = DIRECTION ( 'NONE',  ( -1.000000000000000000, -0.000000000000000000, 0.000000000000000000 ) ) ;
#4492 = EDGE_CURVE ( 'NONE', #3221, #5933, #1204, .T. ) ;
#4493 = CARTESIAN_POINT ( 'NONE',  ( -2.061894914253512123, 6.087690860853031793, 6.857782953271941950E-17 ) ) ;
#4494 = CARTESIAN_POINT ( 'NONE',  ( -10.00000000000000000, 0.000000000000000000, 0.000000000000000000 ) ) ;
#4495 = ADVANCED_FACE ( 'NONE', ( #8166 ), #2417, .T. ) ;
#4496 = AXIS2_PLACEMENT_3D ( 'NONE', #6019, #11413, #3948 ) ;
#4497 = CARTESIAN_POINT ( 'NONE',  ( 0.0002901587068752367257, -4.749354241797645315, 10.00000000000000000 ) ) ;
#4498 = EDGE_LOOP ( 'NONE', ( #2013, #7796 ) ) ;
#4499 = EDGE_CURVE ( 'NONE', #11993, #7265, #5114, .T. ) ;
#4500 = ORIENTED_EDGE ( 'NONE', *, *, #4857, .F. ) ;
#4501 = EDGE_LOOP ( 'NONE', ( #11997, #7492, #11772, #11202 ) ) ;
#4502 = AXIS2_PLACEMENT_3D ( 'NONE', #3643, #12018, #6393 ) ;
#4503 = CARTESIAN_POINT ( 'NONE',  ( -10.19073739998278683, -11.62312336453203798, 10.00000000000000000 ) ) ;
#4504 = AXIS2_PLACEMENT_3D ( 'NONE', #8954, #630, #11825 ) ;
#4505 = CARTESIAN_POINT ( 'NONE',  ( 0.000000000000000000, 12.88318129270179035, 18.51065745848382349 ) ) ;
#4506 = DIRECTION ( 'NONE',  ( 0.000000000000000000, 0.9510565162951544194, -0.3090169943749449533 ) ) ;
#4507 = CARTESIAN_POINT ( 'NONE',  ( 4.623190192904133689, -5.402202315098909580, 3.747395293195558847E-16 ) ) ;
#4508 = AXIS2_PLACEMENT_3D ( 'NONE', #9570, #3145, #8775 ) ;
#4509 = CARTESIAN_POINT ( 'NONE',  ( 3.000000000000000888, -17.31945870441157354, 15.13242714128113775 ) ) ;
#4510 = CIRCLE ( 'NONE', #5094, 9.599999999999997868 ) ;
#4511 = AXIS2_PLACEMENT_3D ( 'NONE', #4551, #1788, #8344 ) ;
#4512 = CYLINDRICAL_SURFACE ( 'NONE', #9965, 24.80000000000000071 ) ;
#4513 = ORIENTED_EDGE ( 'NONE', *, *, #9872, .T. ) ;
#4514 = ORIENTED_EDGE ( 'NONE', *, *, #6325, .T. ) ;
#4515 = COLOUR_RGB ( '', 0.31764706, 0.68627451, 0.89019608) ;
#4516 = VERTEX_POINT ( 'NONE', #10000 ) ;
#4517 = CARTESIAN_POINT ( 'NONE',  ( 0.000000000000000000, -20.93895013827572171, -13.28910708463150492 ) ) ;
#4518 = PLANE ( 'NONE',  #9168 ) ;
#4519 = AXIS2_PLACEMENT_3D ( 'NONE', #2088, #11395, #1967 ) ;
#4520 = AXIS2_PLACEMENT_3D ( 'NONE', #11907, #6226, #2552 ) ;
#4521 = PRODUCT_DEFINITION_CONTEXT ( 'detailed design', #9271, 'design' ) ;
#4522 = DIRECTION ( 'NONE',  ( -1.000000000000000000, 0.000000000000000000, 0.000000000000000000 ) ) ;
#4523 = CIRCLE ( 'NONE', #10179, 9.599999999999996092 ) ;
#4524 = AXIS2_PLACEMENT_3D ( 'NONE', #11608, #10503, #4203 ) ;
#4525 = EDGE_CURVE ( 'NONE', #1487, #8295, #8039, .T. ) ;
#4526 = DIRECTION ( 'NONE',  ( 0.000000000000000000, 0.000000000000000000, -1.000000000000000000 ) ) ;
#4527 = CARTESIAN_POINT ( 'NONE',  ( 3.000000000000000888, 17.06259499759964271, -14.74749645579993995 ) ) ;
#4528 = LINE ( 'NONE', #10145, #11372 ) ;
#4529 = CLOSED_SHELL ( 'NONE', ( #1759, #5007, #6067, #8839, #6656, #1565 ) ) ;
#4530 = CARTESIAN_POINT ( 'NONE',  ( 3.000000000000000888, -0.4575788569253416149, 22.54798042742717712 ) ) ;
#4531 = ORIENTED_EDGE ( 'NONE', *, *, #7268, .F. ) ;
#4532 = FACE_OUTER_BOUND ( 'NONE', #6394, .T. ) ;
#4533 = EDGE_CURVE ( 'NONE', #5043, #1474, #5173, .T. ) ;
#4534 = CIRCLE ( 'NONE', #10982, 19.99999999999999645 ) ;
#4535 = ORIENTED_EDGE ( 'NONE', *, *, #8438, .F. ) ;
#4536 = VERTEX_POINT ( 'NONE', #5230 ) ;
#4537 = B_SPLINE_CURVE_WITH_KNOTS ( 'NONE', 3,
 ( #7637, #349, #10335, #8569, #10400, #9424, #3117, #2131, #9662, #11383, #9602, #233, #3002, #2076, #1045, #4892, #6777, #1954, #7575, #4958, #5813, #5757, #8630, #4774, #293, #9541, #9482, #1221, #8513, #1279, #1156, #167, #3979, #111, #6836, #8695, #7704, #4030, #7758, #10580, #2196, #5936, #5012, #4092, #7822, #11559, #1398, #7941, #2256, #5992, #473, #3233, #5132, #10643, #2435, #9775, #11616, #8926, #7995, #4268, #6900, #7010, #4158, #8982, #5248, #8871, #3181, #11733, #595, #7886, #5191, #11670, #6953, #533, #9717, #1456, #3357, #6113, #1331, #7071, #9901, #5067, #10825, #6174, #413, #4212, #3288, #10697, #8807, #10757, #6047, #2309, #2373, #9846, #1515, #2234, #10679, #9583, #10554, #11477, #4071, #6879, #2291, #272, #10621, #4993, #4014, #3097, #10438, #9641, #7800, #11356, #8610, #9700, #7740, #6815, #2173, #3160, #8785, #5852, #6933, #11537, #2056, #6027, #5914, #11421, #1261, #1135, #7866, #5970, #2980, #1312, #8731, #333, #5048, #391, #9755, #4136, #5794, #11599, #4871, #5106, #3216, #1375, #8850, #9519, #3042, #454, #4194, #6701, #206, #3955, #7682, #6760, #10496, #2112, #1197, #4935, #8672, #11776, #11653, #8907, #10060, #3405, #513, #640, #9089, #9140, #2603, #6272, #4432, #3465, #6091, #2350, #11891, #10985, #4374, #1555, #3269, #10804, #7052, #6991, #2414, #698, #5170, #10736, #9882, #5292, #4248, #10917, #7232, #1679, #7173, #5360, #7920, #7975, #8164, #3520, #1438, #8108, #1624, #11710, #5414, #756, #9822, #11833, #2534, #9998 ),
 .UNSPECIFIED., .F., .F.,
 ( 4, 2, 2, 2, 2, 2, 2, 2, 2, 2, 2, 2, 2, 2, 2, 2, 2, 2, 2, 2, 2, 2, 2, 2, 2, 2, 2, 2, 2, 2, 2, 2, 2, 2, 2, 2, 2, 2, 2, 2, 2, 2, 2, 2, 2, 2, 2, 2, 2, 2, 2, 2, 2, 2, 2, 2, 2, 2, 2, 2, 2, 2, 2, 2, 2, 2, 2, 2, 2, 2, 2, 2, 2, 2, 2, 2, 2, 2, 2, 2, 2, 2, 2, 2, 2, 2, 2, 2, 2, 2, 2, 2, 2, 2, 2, 2, 2, 2, 2, 2, 2, 2, 2, 4 ),
 ( 0.000000000000000000, 0.007812500000000000000, 0.01562500000000000000, 0.02343750000000000000, 0.03125000000000000000, 0.03906250000000000000, 0.04687500000000000000, 0.05468750000000000000, 0.06250000000000000000, 0.07031250000000000000, 0.07812500000000000000, 0.08593750000000000000, 0.09375000000000000000, 0.1015624999999999861, 0.1093750000000000000, 0.1171875000000000000, 0.1250000000000000000, 0.1328125000000000000, 0.1406250000000000000, 0.1484375000000000000, 0.1562500000000000000, 0.1640624999999999722, 0.1718750000000000000, 0.1796875000000000000, 0.1875000000000000000, 0.1953125000000000000, 0.2031249999999999722, 0.2109375000000000000, 0.2187500000000000000, 0.2265625000000000000, 0.2343750000000000000, 0.2421875000000000000, 0.2500000000000000000, 0.2578125000000000000, 0.2656250000000000000, 0.2734375000000000000, 0.2812500000000000000, 0.2890625000000000000, 0.2968750000000000000, 0.3046875000000000000, 0.3125000000000000000, 0.3203125000000000000, 0.3281249999999999445, 0.3359375000000000000, 0.3437500000000000000, 0.3515625000000000000, 0.3593750000000000000, 0.3671874999999999445, 0.3750000000000000000, 0.3828125000000000000, 0.3906250000000000000, 0.3984375000000000000, 0.4062499999999999445, 0.4140625000000000000, 0.4218750000000000000, 0.4296875000000000000, 0.4375000000000000000, 0.4453125000000000000, 0.4531250000000000000, 0.4609375000000000000, 0.4687500000000000000, 0.4765625000000000000, 0.4843750000000000000, 0.4921875000000000000, 0.5000000000000000000, 0.5078125000000000000, 0.5156250000000000000, 0.5234375000000000000, 0.5312500000000000000, 0.5390625000000000000, 0.5468750000000000000, 0.5546875000000000000, 0.5625000000000000000, 0.5703125000000000000, 0.5781250000000000000, 0.5859375000000000000, 0.5937500000000000000, 0.6015625000000000000, 0.6093750000000000000, 0.6171874999999998890, 0.6250000000000000000, 0.6328125000000000000, 0.6406250000000000000, 0.6484375000000000000, 0.6562499999999998890, 0.6640625000000000000, 0.6718750000000000000, 0.6796875000000000000, 0.6875000000000000000, 0.6953124999999998890, 0.7031250000000000000, 0.7109375000000000000, 0.7187500000000000000, 0.7265625000000000000, 0.7343749999999998890, 0.7421875000000000000, 0.7500000000000000000, 0.7656250000000000000, 0.7812500000000000000, 0.7968750000000000000, 0.8124999999999998890, 0.8281250000000000000, 0.8437500000000000000, 0.8499999999999999778 ),
 .UNSPECIFIED. ) ;
#4538 = CARTESIAN_POINT ( 'NONE',  ( 0.5199114366211746718, 8.229807867079658834, 10.00000000000000000 ) ) ;
#4539 = ORIENTED_EDGE ( 'NONE', *, *, #4002, .T. ) ;
#4540 = CYLINDRICAL_SURFACE ( 'NONE', #3054, 24.80000000000000071 ) ;
#4541 = VERTEX_POINT ( 'NONE', #3583 ) ;
#4542 = AXIS2_PLACEMENT_3D ( 'NONE', #11288, #7788, #1251 ) ;
#4543 = AXIS2_PLACEMENT_3D ( 'NONE', #5945, #5882, #5075 ) ;
#4544 = FACE_OUTER_BOUND ( 'NONE', #4266, .T. ) ;
#4545 = DIRECTION ( 'NONE',  ( 0.000000000000000000, 0.9781476007338048007, 0.2079116908177630618 ) ) ;
#4546 = CARTESIAN_POINT ( 'NONE',  ( -10.85385039129052842, -12.37615246896657339, 6.857782953271941950E-17 ) ) ;
#4547 = DIRECTION ( 'NONE',  ( 0.000000000000000000, 0.000000000000000000, 1.000000000000000000 ) ) ;
#4548 = DIRECTION ( 'NONE',  ( 0.000000000000000000, 0.000000000000000000, 1.000000000000000000 ) ) ;
#4549 = VERTEX_POINT ( 'NONE', #6158 ) ;
#4550 = VERTEX_POINT ( 'NONE', #7235 ) ;
#4551 = CARTESIAN_POINT ( 'NONE',  ( 0.000000000000000000, 18.51065745848377730, 12.88318129270185430 ) ) ;
#4552 = ORIENTED_EDGE ( 'NONE', *, *, #2115, .F. ) ;
#4553 = CIRCLE ( 'NONE', #11389, 11.50000000000000178 ) ;
#4554 = CARTESIAN_POINT ( 'NONE',  ( 7.261170810407326037, -1.543028577657243439, 3.747395293195558847E-16 ) ) ;
#4555 = DIRECTION ( 'NONE',  ( -1.000000000000000000, -0.000000000000000000, -0.000000000000000000 ) ) ;
#4556 = DIRECTION ( 'NONE',  ( -1.000000000000000000, -0.000000000000000000, -0.000000000000000000 ) ) ;
#4557 = CARTESIAN_POINT ( 'NONE',  ( 0.000000000000000000, 19.74380051311556628, -11.79560690673851475 ) ) ;
#4558 = DIRECTION ( 'NONE',  ( -1.000000000000000000, -0.000000000000000000, -0.000000000000000000 ) ) ;
#4559 = CARTESIAN_POINT ( 'NONE',  ( 0.6279411196271849072, -4.781877258324066737, 6.857782953271941950E-17 ) ) ;
#4560 = CARTESIAN_POINT ( 'NONE',  ( 1.500000000000000444, -20.65684170206481696, -13.72351598154918406 ) ) ;
#4561 = CARTESIAN_POINT ( 'NONE',  ( 19.00000000000000000, 0.000000000000000000, -5.000000000000000000 ) ) ;
#4562 = ADVANCED_FACE ( 'NONE', ( #7977 ), #8909, .T. ) ;
#4563 = CIRCLE ( 'NONE', #11584, 9.599999999999997868 ) ;
#4564 = AXIS2_PLACEMENT_3D ( 'NONE', #4494, #6212, #5295 ) ;
#4565 = ORIENTED_EDGE ( 'NONE', *, *, #2546, .T. ) ;
#4566 = ORIENTED_EDGE ( 'NONE', *, *, #4966, .F. ) ;
#4567 = AXIS2_PLACEMENT_3D ( 'NONE', #9909, #8991, #10026 ) ;
#4568 = DIRECTION ( 'NONE',  ( 1.000000000000000000, -0.000000000000000000, -0.000000000000000000 ) ) ;
#4569 = CARTESIAN_POINT ( 'NONE',  ( 9.701579622838506722, -3.641351606116563389, 10.00000000000000000 ) ) ;
#4570 = EDGE_CURVE ( 'NONE', #3056, #8295, #806, .T. ) ;
#4571 = DIRECTION ( 'NONE',  ( 0.000000000000000000, 0.000000000000000000, 1.000000000000000000 ) ) ;
#4572 = DIRECTION ( 'NONE',  ( -1.000000000000000000, -0.000000000000000000, -0.000000000000000000 ) ) ;
#4573 = ADVANCED_FACE ( 'NONE', ( #2606 ), #4310, .T. ) ;
#4574 = CARTESIAN_POINT ( 'NONE',  ( -8.457858257354885723, -3.686763380685289970, 3.747395293195558847E-16 ) ) ;
#4575 = CYLINDRICAL_SURFACE ( 'NONE', #10609, 22.99899999999999878 ) ;
#4576 = CIRCLE ( 'NONE', #5155, 9.599999999999997868 ) ;
#4577 = DIRECTION ( 'NONE',  ( -1.000000000000000000, 0.000000000000000000, -0.000000000000000000 ) ) ;
#4578 = ORIENTED_EDGE ( 'NONE', *, *, #2619, .F. ) ;
#4579 = ORIENTED_EDGE ( 'NONE', *, *, #6948, .T. ) ;
#4580 = ORIENTED_EDGE ( 'NONE', *, *, #7558, .F. ) ;
#4581 = VERTEX_POINT ( 'NONE', #700 ) ;
#4582 = EDGE_CURVE ( 'NONE', #9364, #10168, #6341, .T. ) ;
#4583 = CYLINDRICAL_SURFACE ( 'NONE', #9249, 9.599999999999997868 ) ;
#4584 = CARTESIAN_POINT ( 'NONE',  ( 0.07364157424580693168, -3.751631698233777179, 5.000000000000000000 ) ) ;
#4585 = CIRCLE ( 'NONE', #8697, 24.80000000000000071 ) ;
#4586 = CARTESIAN_POINT ( 'NONE',  ( 0.000000000000000000, 19.29833442572375546, -11.67026512804527272 ) ) ;
#4587 = FACE_OUTER_BOUND ( 'NONE', #4829, .T. ) ;
#4588 = CARTESIAN_POINT ( 'NONE',  ( 3.000000000000000888, 0.000000000000000000, 0.000000000000000000 ) ) ;
#4589 = CARTESIAN_POINT ( 'NONE',  ( -9.470608727120474413, 11.15741021143934297, 3.747395293195558847E-16 ) ) ;
#4590 = CARTESIAN_POINT ( 'NONE',  ( 5.247589697392725405, -6.187652788349031319, 6.857782953271941950E-17 ) ) ;
#4591 = ADVANCED_FACE ( 'NONE', ( #11713 ), #5416, .T. ) ;
#4592 = CARTESIAN_POINT ( 'NONE',  ( 0.000000000000000000, 0.000000000000000000, 4.000000000000000000 ) ) ;
#4593 = VECTOR ( 'NONE', #6196, 1000.000000000000000 ) ;
#4594 = VERTEX_POINT ( 'NONE', #11953 ) ;
#4595 = EDGE_LOOP ( 'NONE', ( #7940, #4107, #1110, #7254 ) ) ;
#4596 = CARTESIAN_POINT ( 'NONE',  ( 3.000000000000000888, -18.40266524480579236, -13.79477846460815194 ) ) ;
#4597 = ORIENTED_EDGE ( 'NONE', *, *, #7558, .T. ) ;
#4598 = EDGE_CURVE ( 'NONE', #8541, #6939, #2798, .T. ) ;
#4599 = CARTESIAN_POINT ( 'NONE',  ( 6.841929108544089644, -2.672872603903728717, 10.00000000000000000 ) ) ;
#4600 = ORIENTED_EDGE ( 'NONE', *, *, #11256, .F. ) ;
#4601 = CARTESIAN_POINT ( 'NONE',  ( 0.000000000000000000, 0.000000000000000000, 0.000000000000000000 ) ) ;
#4602 = ORIENTED_EDGE ( 'NONE', *, *, #8757, .F. ) ;
#4603 = FACE_OUTER_BOUND ( 'NONE', #6498, .T. ) ;
#4604 = EDGE_CURVE ( 'NONE', #3976, #1739, #642, .T. ) ;
#4605 = CARTESIAN_POINT ( 'NONE',  ( 3.000000000000000888, -10.87771529938148518, -19.75591328264897228 ) ) ;
#4606 = CARTESIAN_POINT ( 'NONE',  ( -2.570438583093578533, 5.934334910739571534, 10.00000000000000000 ) ) ;
#4607 = CARTESIAN_POINT ( 'NONE',  ( 3.000000000000000888, 21.30300407174362576, -7.402892494506364329 ) ) ;
#4608 = CARTESIAN_POINT ( 'NONE',  ( 0.000000000000000000, 0.000000000000000000, 0.000000000000000000 ) ) ;
#4609 = VERTEX_POINT ( 'NONE', #1440 ) ;
#4610 = VERTEX_POINT ( 'NONE', #11837 ) ;
#4611 = DIRECTION ( 'NONE',  ( -1.000000000000000000, 0.000000000000000000, 0.000000000000000000 ) ) ;
#4612 = ORIENTED_EDGE ( 'NONE', *, *, #7713, .F. ) ;
#4613 = AXIS2_PLACEMENT_3D ( 'NONE', #882, #4555, #3577 ) ;
#4614 = CARTESIAN_POINT ( 'NONE',  ( -5.846204292276366843, 1.022993486932169516, 3.747395293195558847E-16 ) ) ;
#4615 = DIRECTION ( 'NONE',  ( -1.000000000000000000, -0.000000000000000000, -0.000000000000000000 ) ) ;
#4616 =( NAMED_UNIT ( * ) SI_UNIT ( $, .STERADIAN. ) SOLID_ANGLE_UNIT ( ) );
#4617 = DIRECTION ( 'NONE',  ( 0.000000000000000000, 0.000000000000000000, 1.000000000000000000 ) ) ;
#4618 = DIRECTION ( 'NONE',  ( 0.000000000000000000, 0.000000000000000000, 1.000000000000000000 ) ) ;
#4619 = DIRECTION ( 'NONE',  ( 0.000000000000000000, 0.000000000000000000, 1.000000000000000000 ) ) ;
#4620 = VECTOR ( 'NONE', #2037, 1000.000000000000000 ) ;
#4621 = MANIFOLD_SOLID_BREP ( 'Sweep1', #6859 ) ;
#4622 = CARTESIAN_POINT ( 'NONE',  ( 1.022653496104248605, 6.171874473422422902, 6.857782953271941950E-17 ) ) ;
#4623 = DIRECTION ( 'NONE',  ( 0.000000000000000000, 0.000000000000000000, 1.000000000000000000 ) ) ;
#4624 = CARTESIAN_POINT ( 'NONE',  ( 3.000000000000000888, -22.37663021667341923, -2.811977935938010376 ) ) ;
#4625 = ORIENTED_EDGE ( 'NONE', *, *, #3474, .F. ) ;
#4626 = EDGE_LOOP ( 'NONE', ( #3325, #6065, #4828, #9068 ) ) ;
#4627 = VECTOR ( 'NONE', #11501, 1000.000000000000000 ) ;
#4628 = DIRECTION ( 'NONE',  ( -1.000000000000000000, 0.000000000000000000, -0.000000000000000000 ) ) ;
#4629 = CARTESIAN_POINT ( 'NONE',  ( -4.046710180314750716, 10.72208681399755648, 10.00000000000000000 ) ) ;
#4630 = LINE ( 'NONE', #8173, #948 ) ;
#4631 = DIRECTION ( 'NONE',  ( 0.000000000000000000, 0.000000000000000000, 1.000000000000000000 ) ) ;
#4632 = CARTESIAN_POINT ( 'NONE',  ( 4.583115687978880359, -8.898851689028539624, 3.747395293195558847E-16 ) ) ;
#4633 = CARTESIAN_POINT ( 'NONE',  ( 0.07364157424580704270, -3.751631698233870438, 3.747395293195558847E-16 ) ) ;
#4634 = LINE ( 'NONE', #7372, #9985 ) ;
#4635 = ORIENTED_EDGE ( 'NONE', *, *, #134, .F. ) ;
#4636 = EDGE_CURVE ( 'NONE', #662, #3166, #1431, .T. ) ;
#4637 = ORIENTED_EDGE ( 'NONE', *, *, #1063, .T. ) ;
#4638 = ADVANCED_FACE ( 'NONE', ( #6451 ), #5597, .T. ) ;
#4639 = EDGE_CURVE ( 'NONE', #531, #11364, #449, .T. ) ;
#4640 = EDGE_LOOP ( 'NONE', ( #791, #2239, #11508, #9729 ) ) ;
#4641 = CARTESIAN_POINT ( 'NONE',  ( 3.000000000000000888, -22.37663021667346186, 2.811977935937707063 ) ) ;
#4642 = CARTESIAN_POINT ( 'NONE',  ( 3.000000000000000888, -15.64281154287585807, -16.85990652506916021 ) ) ;
#4643 = DIRECTION ( 'NONE',  ( -1.000000000000000000, -0.000000000000000000, 0.000000000000000000 ) ) ;
#4644 = CARTESIAN_POINT ( 'NONE',  ( 3.000000000000000888, -13.62355943574031869, 17.97274125076070206 ) ) ;
#4645 = DIRECTION ( 'NONE',  ( 0.000000000000000000, 0.000000000000000000, 1.000000000000000000 ) ) ;
#4646 = CARTESIAN_POINT ( 'NONE',  ( 0.2599977045009999599, -15.80854529698373589, 3.747395293195558847E-16 ) ) ;
#4647 = CARTESIAN_POINT ( 'NONE',  ( -3.542987847618818353, 5.503081486278154522, 6.857782953271941950E-17 ) ) ;
#4648 = EDGE_CURVE ( 'NONE', #4226, #5406, #7684, .T. ) ;
#4649 = EDGE_CURVE ( 'NONE', #10066, #11319, #5470, .T. ) ;
#4650 = CARTESIAN_POINT ( 'NONE',  ( 3.000000000000000888, 0.000000000000000000, 0.000000000000000000 ) ) ;
#4651 = EDGE_LOOP ( 'NONE', ( #10157, #11839, #8085, #11614 ) ) ;
#4652 = VECTOR ( 'NONE', #7678, 1000.000000000000000 ) ;
#4653 = VERTEX_POINT ( 'NONE', #8292 ) ;
#4654 = CARTESIAN_POINT ( 'NONE',  ( 3.000000000000000888, -21.97702544527753332, -6.779701584702958250 ) ) ;
#4655 = ORIENTED_EDGE ( 'NONE', *, *, #11376, .T. ) ;
#4656 = AXIS2_PLACEMENT_3D ( 'NONE', #554, #9920, #7216 ) ;
#4657 = VERTEX_POINT ( 'NONE', #4680 ) ;
#4658 = CARTESIAN_POINT ( 'NONE',  ( -7.228014483236704444E-17, 0.5000000000000005551, 3.000000000000000000 ) ) ;
#4659 = PLANE ( 'NONE',  #9705 ) ;
#4660 = ORIENTED_EDGE ( 'NONE', *, *, #3754, .F. ) ;
#4661 = DIRECTION ( 'NONE',  ( 0.000000000000000000, 0.8090169943749445647, 0.5877852522924771339 ) ) ;
#4662 = DIRECTION ( 'NONE',  ( -1.000000000000000000, 0.000000000000000000, 0.000000000000000000 ) ) ;
#4663 = CARTESIAN_POINT ( 'NONE',  ( -5.248573321596930796, 4.168074790661433049, 10.00000000000000000 ) ) ;
#4664 = CIRCLE ( 'NONE', #2908, 9.599999999999997868 ) ;
#4665 = AXIS2_PLACEMENT_3D ( 'NONE', #464, #2300, #11788 ) ;
#4666 = CARTESIAN_POINT ( 'NONE',  ( 50.00005079999999680, 0.000000000000000000, 0.000000000000000000 ) ) ;
#4667 = DIRECTION ( 'NONE',  ( 0.000000000000000000, 0.000000000000000000, 1.000000000000000000 ) ) ;
#4668 = DIRECTION ( 'NONE',  ( -1.000000000000000000, -0.000000000000000000, -0.000000000000000000 ) ) ;
#4669 = ORIENTED_EDGE ( 'NONE', *, *, #771, .T. ) ;
#4670 = LINE ( 'NONE', #7472, #1971 ) ;
#4671 = EDGE_LOOP ( 'NONE', ( #4725, #3238, #7526, #9497 ) ) ;
#4672 = CARTESIAN_POINT ( 'NONE',  ( -1.035167565893234443, -12.71157708251009488, 10.00000000000000000 ) ) ;
#4673 = CARTESIAN_POINT ( 'NONE',  ( 0.000000000000000000, 0.000000000000000000, 20.00000000000000000 ) ) ;
#4674 =( NAMED_UNIT ( * ) SI_UNIT ( $, .STERADIAN. ) SOLID_ANGLE_UNIT ( ) );
#4675 = DIRECTION ( 'NONE',  ( 1.000000000000000000, 0.000000000000000000, 0.000000000000000000 ) ) ;
#4676 = CARTESIAN_POINT ( 'NONE',  ( 1.500000000000000444, 15.40502424595171149, -19.43515443678387200 ) ) ;
#4677 = CARTESIAN_POINT ( 'NONE',  ( 7.014224211608842907, -15.49593329755746929, 10.00000000000000000 ) ) ;
#4678 = EDGE_CURVE ( 'NONE', #11323, #1657, #10361, .T. ) ;
#4679 = CARTESIAN_POINT ( 'NONE',  ( -6.661525743073264394, 1.789546221321740793, 6.857782953271941950E-17 ) ) ;
#4680 = CARTESIAN_POINT ( 'NONE',  ( 1.500000000000000222, 0.000000000000000000, 0.000000000000000000 ) ) ;
#4681 = CIRCLE ( 'NONE', #9562, 22.99899999999999878 ) ;
#4682 = CARTESIAN_POINT ( 'NONE',  ( 3.000000000000000888, 1.901833551798570721, -22.47229024614975401 ) ) ;
#4683 = ORIENTED_EDGE ( 'NONE', *, *, #12031, .T. ) ;
#4684 = VERTEX_POINT ( 'NONE', #8415 ) ;
#4685 = EDGE_CURVE ( 'NONE', #8902, #5976, #6505, .T. ) ;
#4686 = VERTEX_POINT ( 'NONE', #2719 ) ;
#4687 = DIRECTION ( 'NONE',  ( -1.000000000000000000, 0.000000000000000000, -0.000000000000000000 ) ) ;
#4688 = CARTESIAN_POINT ( 'NONE',  ( -0.1481022647113163504, -9.773457036294484368, 10.00000000000000000 ) ) ;
#4689 = AXIS2_PLACEMENT_3D ( 'NONE', #8621, #221, #3966 ) ;
#4690 = CARTESIAN_POINT ( 'NONE',  ( 3.000000000000000888, -6.779701584702581663, -21.97702544527764701 ) ) ;
#4691 = LINE ( 'NONE', #12085, #8964 ) ;
#4692 = AXIS2_PLACEMENT_3D ( 'NONE', #10822, #1274, #5245 ) ;
#4693 = CARTESIAN_POINT ( 'NONE',  ( -7.812220363925484357, -5.053636123081432174, 3.747395293195558847E-16 ) ) ;
#4694 = DIRECTION ( 'NONE',  ( 0.000000000000000000, -0.1045284632676607012, 0.9945218953682726237 ) ) ;
#4695 = DIRECTION ( 'NONE',  ( -1.000000000000000000, -0.000000000000000000, 0.000000000000000000 ) ) ;
#4696 = ORIENTED_EDGE ( 'NONE', *, *, #2962, .T. ) ;
#4697 = AXIS2_PLACEMENT_3D ( 'NONE', #6276, #2353, #5231 ) ;
#4698 = ORIENTED_EDGE ( 'NONE', *, *, #15, .T. ) ;
#4699 = EDGE_LOOP ( 'NONE', ( #4790, #6783, #10293, #8981 ) ) ;
#4700 = AXIS2_PLACEMENT_3D ( 'NONE', #7308, #7249, #4805 ) ;
#4701 = ORIENTED_EDGE ( 'NONE', *, *, #1157, .F. ) ;
#4702 = CARTESIAN_POINT ( 'NONE',  ( 0.000000000000000000, 22.37663021667344054, -2.811977935937859385 ) ) ;
#4703 = CARTESIAN_POINT ( 'NONE',  ( 0.000000000000000000, 0.000000000000000000, 0.000000000000000000 ) ) ;
#4704 = CARTESIAN_POINT ( 'NONE',  ( 8.000000000000000000, 0.000000000000000000, 0.000000000000000000 ) ) ;
#4705 = DIRECTION ( 'NONE',  ( 0.000000000000000000, 0.000000000000000000, 1.000000000000000000 ) ) ;
#4706 = VECTOR ( 'NONE', #8599, 1000.000000000000000 ) ;
#4707 = CARTESIAN_POINT ( 'NONE',  ( 0.000000000000000000, 14.74749645580034496, -17.06259499759930165 ) ) ;
#4708 = AXIS2_PLACEMENT_3D ( 'NONE', #4281, #10709, #3373 ) ;
#4709 = VECTOR ( 'NONE', #5281, 1000.000000000000000 ) ;
#4710 = CARTESIAN_POINT ( 'NONE',  ( 7.983652613117083519, -10.39416588708253819, 3.747395293195558847E-16 ) ) ;
#4711 = CARTESIAN_POINT ( 'NONE',  ( 3.000000000000000888, -22.54798042742717357, -0.4575788569254196636 ) ) ;
#4712 = PRESENTATION_LAYER_ASSIGNMENT (  '', '', ( #5483 ) ) ;
#4713 = CARTESIAN_POINT ( 'NONE',  ( -1.500000000000000222, 1.836970198721030181E-16, 4.000000000000000000 ) ) ;
#4714 = EDGE_CURVE ( 'NONE', #3630, #3600, #6322, .T. ) ;
#4715 = ORIENTED_EDGE ( 'NONE', *, *, #5957, .T. ) ;
#4716 = ORIENTED_EDGE ( 'NONE', *, *, #682, .T. ) ;
#4717 = DIRECTION ( 'NONE',  ( 1.000000000000000000, -0.000000000000000000, -0.000000000000000000 ) ) ;
#4718 = ORIENTED_EDGE ( 'NONE', *, *, #11621, .F. ) ;
#4719 = AXIS2_PLACEMENT_3D ( 'NONE', #5487, #5610, #3653 ) ;
#4720 = VERTEX_POINT ( 'NONE', #1921 ) ;
#4721 = CARTESIAN_POINT ( 'NONE',  ( 3.000000000000000888, 0.000000000000000000, 0.000000000000000000 ) ) ;
#4722 = AXIS2_PLACEMENT_3D ( 'NONE', #674, #613, #3246 ) ;
#4723 = EDGE_CURVE ( 'NONE', #4242, #3460, #8861, .T. ) ;
#4724 = CARTESIAN_POINT ( 'NONE',  ( 0.000000000000000000, -13.79477846460783574, -18.40266524480602683 ) ) ;
#4725 = ORIENTED_EDGE ( 'NONE', *, *, #1223, .F. ) ;
#4726 = EDGE_CURVE ( 'NONE', #4299, #7424, #3586, .T. ) ;
#4727 = CYLINDRICAL_SURFACE ( 'NONE', #5735, 22.99899999999999878 ) ;
#4728 = EDGE_CURVE ( 'NONE', #9467, #9480, #9050, .T. ) ;
#4729 = CYLINDRICAL_SURFACE ( 'NONE', #1025, 24.80000000000000071 ) ;
#4730 = CARTESIAN_POINT ( 'NONE',  ( 16.47843063274904196, -5.593696103119284224, 6.857782953271941950E-17 ) ) ;
#4731 = CIRCLE ( 'NONE', #5288, 22.99899999999999523 ) ;
#4732 = DIRECTION ( 'NONE',  ( -0.9973083954695386444, 0.07332096784668425127, 7.625284521749261502E-18 ) ) ;
#4733 = AXIS2_PLACEMENT_3D ( 'NONE', #4711, #9417, #2352 ) ;
#4734 = DIRECTION ( 'NONE',  ( -1.000000000000000000, 0.000000000000000000, -0.000000000000000000 ) ) ;
#4735 = VERTEX_POINT ( 'NONE', #9450 ) ;
#4736 = DIRECTION ( 'NONE',  ( -1.000000000000000000, 0.000000000000000000, -0.000000000000000000 ) ) ;
#4737 = ORIENTED_EDGE ( 'NONE', *, *, #6912, .F. ) ;
#4738 = CARTESIAN_POINT ( 'NONE',  ( 4.123629756450001516, -15.38522696314584870, 10.00000000000000000 ) ) ;
#4739 = DIRECTION ( 'NONE',  ( 0.000000000000000000, 0.8660254037844363761, 0.5000000000000039968 ) ) ;
#4740 = CARTESIAN_POINT ( 'NONE',  ( 3.000000000000000000, 0.000000000000000000, -15.00000000000000000 ) ) ;
#4741 = CARTESIAN_POINT ( 'NONE',  ( -10.00000000000000000, 0.000000000000000000, 0.000000000000000000 ) ) ;
#4742 = CARTESIAN_POINT ( 'NONE',  ( -5.683926142426734884, 14.39978054689284193, 10.00000000000000000 ) ) ;
#4743 = CARTESIAN_POINT ( 'NONE',  ( 4.346347989803176937, 4.041826679702269942, 6.857782953271941950E-17 ) ) ;
#4744 = DIRECTION ( 'NONE',  ( 0.000000000000000000, 0.000000000000000000, 1.000000000000000000 ) ) ;
#4745 = AXIS2_PLACEMENT_3D ( 'NONE', #9370, #2947, #176 ) ;
#4746 = ADVANCED_FACE ( 'NONE', ( #10116 ), #80, .T. ) ;
#4747 = ORIENTED_EDGE ( 'NONE', *, *, #11747, .F. ) ;
#4748 = DIRECTION ( 'NONE',  ( 0.000000000000000000, 0.000000000000000000, -1.000000000000000000 ) ) ;
#4749 = CIRCLE ( 'NONE', #436, 9.599999999999996092 ) ;
#4750 = EDGE_LOOP ( 'NONE', ( #6630, #4747, #2137, #5742 ) ) ;
#4751 = ADVANCED_FACE ( 'NONE', ( #12074 ), #3765, .T. ) ;
#4752 = DIRECTION ( 'NONE',  ( 0.000000000000000000, 0.000000000000000000, 1.000000000000000000 ) ) ;
#4753 = CARTESIAN_POINT ( 'NONE',  ( -8.457858257355617582, -3.686763380685291747, 10.00000000000000000 ) ) ;
#4754 = CIRCLE ( 'NONE', #6691, 4.000000000000000000 ) ;
#4755 = DIRECTION ( 'NONE',  ( 0.000000000000000000, 0.000000000000000000, 1.000000000000000000 ) ) ;
#4756 = CARTESIAN_POINT ( 'NONE',  ( -2.487495860704069361, -9.331140650584718088, 3.747395293195558847E-16 ) ) ;
#4757 = AXIS2_PLACEMENT_3D ( 'NONE', #9937, #9031, #11048 ) ;
#4758 = EDGE_CURVE ( 'NONE', #8246, #11319, #10612, .T. ) ;
#4759 = CARTESIAN_POINT ( 'NONE',  ( 0.000000000000000000, -20.86861857134728027, -9.667200211210033700 ) ) ;
#4760 = ORIENTED_EDGE ( 'NONE', *, *, #11236, .F. ) ;
#4761 = ORIENTED_EDGE ( 'NONE', *, *, #10243, .T. ) ;
#4762 = AXIS2_PLACEMENT_3D ( 'NONE', #10162, #3678, #4661 ) ;
#4763 = ORIENTED_EDGE ( 'NONE', *, *, #90, .T. ) ;
#4764 = ORIENTED_EDGE ( 'NONE', *, *, #7122, .F. ) ;
#4765 = DIRECTION ( 'NONE',  ( -1.000000000000000000, 0.000000000000000000, 0.000000000000000000 ) ) ;
#4766 = CARTESIAN_POINT ( 'NONE',  ( 3.000000000000000888, 0.000000000000000000, 0.000000000000000000 ) ) ;
#4767 = DIRECTION ( 'NONE',  ( 0.000000000000000000, 0.1045284632676471287, 0.9945218953682740670 ) ) ;
#4768 = FACE_OUTER_BOUND ( 'NONE', #6833, .T. ) ;
#4769 = DIRECTION ( 'NONE',  ( 1.000000000000000000, 0.000000000000000000, 0.000000000000000000 ) ) ;
#4770 = CARTESIAN_POINT ( 'NONE',  ( 13.53515989517831564, -0.2218654272304620700, 3.747395293195558847E-16 ) ) ;
#4771 = DIRECTION ( 'NONE',  ( -1.000000000000000000, 0.000000000000000000, 0.000000000000000000 ) ) ;
#4772 = ORIENTED_EDGE ( 'NONE', *, *, #6882, .F. ) ;
#4773 = ORIENTED_EDGE ( 'NONE', *, *, #11442, .F. ) ;
#4774 = CARTESIAN_POINT ( 'NONE',  ( -15.18624859168667918, -5.715447929355455869, 10.00000000000000000 ) ) ;
#4775 = VERTEX_POINT ( 'NONE', #11521 ) ;
#4776 = AXIS2_PLACEMENT_3D ( 'NONE', #3638, #7354, #7417 ) ;
#4777 = CARTESIAN_POINT ( 'NONE',  ( 0.000000000000000000, 0.000000000000000000, 0.000000000000000000 ) ) ;
#4778 = CYLINDRICAL_SURFACE ( 'NONE', #9112, 19.00000000000000000 ) ;
#4779 = ORIENTED_EDGE ( 'NONE', *, *, #10108, .F. ) ;
#4780 = DIRECTION ( 'NONE',  ( 0.000000000000000000, 0.000000000000000000, 1.000000000000000000 ) ) ;
#4781 = DIRECTION ( 'NONE',  ( -1.000000000000000000, 0.000000000000000000, 0.000000000000000000 ) ) ;
#4782 = CARTESIAN_POINT ( 'NONE',  ( -11.39998097177137026, 5.856612080558655897, 6.857782953271941950E-17 ) ) ;
#4783 = AXIS2_PLACEMENT_3D ( 'NONE', #1299, #3315, #7786 ) ;
#4784 = DIRECTION ( 'NONE',  ( 0.000000000000000000, 0.000000000000000000, 1.000000000000000000 ) ) ;
#4785 = CYLINDRICAL_SURFACE ( 'NONE', #5511, 24.80000000000000071 ) ;
#4786 = ORIENTED_EDGE ( 'NONE', *, *, #8969, .T. ) ;
#4787 = EDGE_LOOP ( 'NONE', ( #6187, #6468, #50, #11235 ) ) ;
#4788 = CARTESIAN_POINT ( 'NONE',  ( 3.000000000000000888, -2.062268319295719632, 22.90635393027945454 ) ) ;
#4789 = ADVANCED_FACE ( 'NONE', ( #6865 ), #6925, .T. ) ;
#4790 = ORIENTED_EDGE ( 'NONE', *, *, #6608, .T. ) ;
#4791 = EDGE_CURVE ( 'NONE', #1383, #4254, #8596, .T. ) ;
#4792 = EDGE_CURVE ( 'NONE', #6834, #7011, #3206, .T. ) ;
#4793 = CARTESIAN_POINT ( 'NONE',  ( -14.61026919807147451, 3.159152207411757285, 10.00000000000000000 ) ) ;
#4794 = DIRECTION ( 'NONE',  ( 0.000000000000000000, 0.000000000000000000, -1.000000000000000000 ) ) ;
#4795 = SHAPE_REPRESENTATION_RELATIONSHIP ( 'NONE' , 'NONE' ,  #6698, #1326 ) ;
#4796 = LINE ( 'NONE', #8592, #8762 ) ;
#4797 = FACE_OUTER_BOUND ( 'NONE', #83, .T. ) ;
#4798 = CARTESIAN_POINT ( 'NONE',  ( -0.3972327064967878796, 12.29993208790120640, 10.00000000000000000 ) ) ;
#4799 = CARTESIAN_POINT ( 'NONE',  ( 3.000000000000000888, 21.58580335785685378, -6.532525787310757615 ) ) ;
#4800 = DIRECTION ( 'NONE',  ( 0.000000000000000000, -0.8660254037844328234, -0.5000000000000099920 ) ) ;
#4801 = CARTESIAN_POINT ( 'NONE',  ( -5.101271054653079950, -15.85638610327790765, 6.857782953271941950E-17 ) ) ;
#4802 = EDGE_CURVE ( 'NONE', #10265, #8647, #3384, .T. ) ;
#4803 = DIRECTION ( 'NONE',  ( -1.000000000000000000, 0.000000000000000000, 0.000000000000000000 ) ) ;
#4804 = ORIENTED_EDGE ( 'NONE', *, *, #748, .T. ) ;
#4805 = DIRECTION ( 'NONE',  ( 0.000000000000000000, 0.000000000000000000, 1.000000000000000000 ) ) ;
#4806 = ORIENTED_EDGE ( 'NONE', *, *, #6144, .T. ) ;
#4807 = DIRECTION ( 'NONE',  ( -1.000000000000000000, 0.000000000000000000, 0.000000000000000000 ) ) ;
#4808 = CARTESIAN_POINT ( 'NONE',  ( 8.913847851856345983, -5.129921849437908854, 10.00000000000000000 ) ) ;
#4809 = DIRECTION ( 'NONE',  ( 0.000000000000000000, 0.000000000000000000, 1.000000000000000000 ) ) ;
#4810 = EDGE_CURVE ( 'NONE', #7795, #2848, #1303, .T. ) ;
#4811 = AXIS2_PLACEMENT_3D ( 'NONE', #7777, #3135, #5150 ) ;
#4812 = CARTESIAN_POINT ( 'NONE',  ( -0.1481022647113159063, -9.773457036294480815, 3.747395293195558847E-16 ) ) ;
#4813 = CARTESIAN_POINT ( 'NONE',  ( 0.5005346673319864825, 15.27733729710887545, 6.857782953271941950E-17 ) ) ;
#4814 = EDGE_CURVE ( 'NONE', #518, #1487, #5143, .T. ) ;
#4815 = CARTESIAN_POINT ( 'NONE',  ( 3.000000000000000888, 9.589108953448178596, -20.41249101028201451 ) ) ;
#4816 = ORIENTED_EDGE ( 'NONE', *, *, #4113, .F. ) ;
#4817 = VERTEX_POINT ( 'NONE', #3946 ) ;
#4818 = CIRCLE ( 'NONE', #3064, 9.599999999999996092 ) ;
#4819 = EDGE_LOOP ( 'NONE', ( #5524, #5943, #8943, #6929 ) ) ;
#4820 = FACE_OUTER_BOUND ( 'NONE', #10088, .T. ) ;
#4821 = CARTESIAN_POINT ( 'NONE',  ( 0.000000000000000000, -18.51065745848368849, -12.88318129270198042 ) ) ;
#4822 = DIRECTION ( 'NONE',  ( -1.000000000000000000, 0.000000000000000000, 0.000000000000000000 ) ) ;
#4823 = CARTESIAN_POINT ( 'NONE',  ( 0.000000000000000000, 22.99643626497956816, -0.3433949777332470088 ) ) ;
#4824 = CARTESIAN_POINT ( 'NONE',  ( 0.000000000000000000, -22.56530478845645860, -4.445336973061090546 ) ) ;
#4825 = CARTESIAN_POINT ( 'NONE',  ( -1.872083171988683015, 14.23747171912756038, 3.747395293195558847E-16 ) ) ;
#4826 = ADVANCED_FACE ( 'NONE', ( #2225 ), #6595, .F. ) ;
#4827 = CARTESIAN_POINT ( 'NONE',  ( 3.000000000000000888, -6.668524164681794097, 23.88662356770113249 ) ) ;
#4828 = ORIENTED_EDGE ( 'NONE', *, *, #11375, .F. ) ;
#4829 = EDGE_LOOP ( 'NONE', ( #7035, #6097, #11492, #9437 ) ) ;
#4830 = CARTESIAN_POINT ( 'NONE',  ( 0.000000000000000000, 0.000000000000000000, 0.000000000000000000 ) ) ;
#4831 = CARTESIAN_POINT ( 'NONE',  ( 3.000000000000000888, 18.40266524480588473, 13.79477846460802226 ) ) ;
#4832 = EDGE_LOOP ( 'NONE', ( #2207, #6692, #695, #3047 ) ) ;
#4833 = DIRECTION ( 'NONE',  ( 0.000000000000000000, 0.2079116908177598144, -0.9781476007338055778 ) ) ;
#4834 = EDGE_CURVE ( 'NONE', #9694, #518, #10817, .T. ) ;
#4835 = CARTESIAN_POINT ( 'NONE',  ( -10.00000000000000000, 0.000000000000000000, 0.000000000000000000 ) ) ;
#4836 = VERTEX_POINT ( 'NONE', #1956 ) ;
#4837 = CARTESIAN_POINT ( 'NONE',  ( 0.000000000000000000, 0.000000000000000000, -5.000000000000000000 ) ) ;
#4838 = DIRECTION ( 'NONE',  ( -1.000000000000000000, 0.000000000000000000, 0.000000000000000000 ) ) ;
#4839 = CARTESIAN_POINT ( 'NONE',  ( 14.54887842078032278, 0.9530482589069305677, 6.857782953271941950E-17 ) ) ;
#4840 = CARTESIAN_POINT ( 'NONE',  ( 0.000000000000000000, 0.000000000000000000, 10.00000000000000000 ) ) ;
#4841 = DIRECTION ( 'NONE',  ( -1.000000000000000000, -0.000000000000000000, -0.000000000000000000 ) ) ;
#4842 = AXIS2_PLACEMENT_3D ( 'NONE', #6684, #5592, #5836 ) ;
#4843 = ORIENTED_EDGE ( 'NONE', *, *, #6870, .F. ) ;
#4844 = ORIENTED_EDGE ( 'NONE', *, *, #4038, .F. ) ;
#4845 = CARTESIAN_POINT ( 'NONE',  ( 3.000000000000000888, -21.96011696265495061, 5.135568396239952982 ) ) ;
#4846 = VERTEX_POINT ( 'NONE', #1160 ) ;
#4847 = CARTESIAN_POINT ( 'NONE',  ( 7.983652613117085295, -10.39416588708253997, 10.00000000000000000 ) ) ;
#4848 = CARTESIAN_POINT ( 'NONE',  ( 3.000000000000000888, 0.000000000000000000, 0.000000000000000000 ) ) ;
#4849 = SURFACE_STYLE_USAGE ( .BOTH. , #1975 ) ;
#4850 = CARTESIAN_POINT ( 'NONE',  ( 15.92723891616420673, -6.911623607273379655, 6.857782953271941950E-17 ) ) ;
#4851 = AXIS2_PLACEMENT_3D ( 'NONE', #6359, #5255, #8989 ) ;
#4852 = LINE ( 'NONE', #8350, #6023 ) ;
#4853 = CARTESIAN_POINT ( 'NONE',  ( 3.000000000000000888, 0.000000000000000000, 0.000000000000000000 ) ) ;
#4854 = CARTESIAN_POINT ( 'NONE',  ( -1.410059164928063380, 12.26527237696110184, 10.00000000000000000 ) ) ;
#4855 = DIRECTION ( 'NONE',  ( -1.000000000000000000, 0.000000000000000000, 0.000000000000000000 ) ) ;
#4856 = CARTESIAN_POINT ( 'NONE',  ( -7.115032382426029756, -13.85544350050026452, 3.747395293195558847E-16 ) ) ;
#4857 = EDGE_CURVE ( 'NONE', #4775, #2104, #1629, .T. ) ;
#4858 = DIRECTION ( 'NONE',  ( -1.000000000000000000, 0.000000000000000000, 0.000000000000000000 ) ) ;
#4859 = ORIENTED_EDGE ( 'NONE', *, *, #9298, .T. ) ;
#4860 = FACE_OUTER_BOUND ( 'NONE', #123, .T. ) ;
#4861 = AXIS2_PLACEMENT_3D ( 'NONE', #5372, #6349, #5305 ) ;
#4862 = EDGE_CURVE ( 'NONE', #8329, #10038, #3192, .T. ) ;
#4863 = VECTOR ( 'NONE', #6459, 1000.000000000000000 ) ;
#4864 = ORIENTED_EDGE ( 'NONE', *, *, #2091, .T. ) ;
#4865 = EDGE_LOOP ( 'NONE', ( #10925, #7471, #7238, #5052 ) ) ;
#4866 = LINE ( 'NONE', #8604, #5000 ) ;
#4867 = CARTESIAN_POINT ( 'NONE',  ( 6.841929108544089644, -2.672872603903728717, 10.00000000000000000 ) ) ;
#4868 = EDGE_CURVE ( 'NONE', #1881, #8050, #9484, .T. ) ;
#4869 = DIRECTION ( 'NONE',  ( 0.000000000000000000, 0.000000000000000000, 1.000000000000000000 ) ) ;
#4870 = EDGE_CURVE ( 'NONE', #8517, #2790, #2824, .T. ) ;
#4871 = CARTESIAN_POINT ( 'NONE',  ( -1.672018190274039418, 9.216430685901391584, 10.00000000000000000 ) ) ;
#4872 = AXIS2_PLACEMENT_3D ( 'NONE', #8974, #584, #4321 ) ;
#4873 = CARTESIAN_POINT ( 'NONE',  ( 14.54887842078032278, 0.9530482589069305677, 6.857782953271941950E-17 ) ) ;
#4874 = EDGE_CURVE ( 'NONE', #8071, #9845, #9837, .T. ) ;
#4875 = DIRECTION ( 'NONE',  ( -1.000000000000000000, 0.000000000000000000, 0.000000000000000000 ) ) ;
#4876 = ORIENTED_EDGE ( 'NONE', *, *, #4726, .T. ) ;
#4877 = ORIENTED_EDGE ( 'NONE', *, *, #11554, .F. ) ;
#4878 = AXIS2_PLACEMENT_3D ( 'NONE', #12037, #10267, #8373 ) ;
#4879 = FACE_OUTER_BOUND ( 'NONE', #58, .T. ) ;
#4880 = AXIS2_PLACEMENT_3D ( 'NONE', #2726, #1518, #11108 ) ;
#4881 = CARTESIAN_POINT ( 'NONE',  ( -3.562082835880472587, -15.28349083755603743, 10.00000000000000000 ) ) ;
#4882 = CIRCLE ( 'NONE', #5463, 19.00000000000000000 ) ;
#4883 = ORIENTED_EDGE ( 'NONE', *, *, #5385, .F. ) ;
#4884 = CARTESIAN_POINT ( 'NONE',  ( 0.000000000000000000, 17.06259499759964271, -14.74749645579993995 ) ) ;
#4885 = CARTESIAN_POINT ( 'NONE',  ( 0.000000000000000000, 22.21333432029578603, -11.02759168516723065 ) ) ;
#4886 = DIRECTION ( 'NONE',  ( -1.000000000000000000, 0.000000000000000000, 0.000000000000000000 ) ) ;
#4887 = CARTESIAN_POINT ( 'NONE',  ( -11.74902089294173457, -3.156991809147609906, 3.747395293195558847E-16 ) ) ;
#4888 = AXIS2_PLACEMENT_3D ( 'NONE', #11469, #1186, #3149 ) ;
#4889 = FACE_OUTER_BOUND ( 'NONE', #524, .T. ) ;
#4890 = EDGE_LOOP ( 'NONE', ( #9703, #2879, #4351, #860 ) ) ;
#4891 = ORIENTED_EDGE ( 'NONE', *, *, #134, .T. ) ;
#4892 = CARTESIAN_POINT ( 'NONE',  ( -3.791520748785662587, -16.26028641251513207, 10.00000000000000000 ) ) ;
#4893 = ORIENTED_EDGE ( 'NONE', *, *, #973, .F. ) ;
#4894 = CARTESIAN_POINT ( 'NONE',  ( 3.000000000000000888, 21.97817939804055598, -11.48910920600660646 ) ) ;
#4895 = LINE ( 'NONE', #3982, #11600 ) ;
#4896 = AXIS2_PLACEMENT_3D ( 'NONE', #8293, #6453, #6749 ) ;
#4897 = EDGE_CURVE ( 'NONE', #9669, #8183, #113, .T. ) ;
#4898 = DIRECTION ( 'NONE',  ( 0.000000000000000000, 0.000000000000000000, 1.000000000000000000 ) ) ;
#4899 = ORIENTED_EDGE ( 'NONE', *, *, #9824, .F. ) ;
#4900 = AXIS2_PLACEMENT_3D ( 'NONE', #8648, #3869, #8763 ) ;
#4901 = DIRECTION ( 'NONE',  ( 0.000000000000000000, 0.000000000000000000, -1.000000000000000000 ) ) ;
#4902 =( GEOMETRIC_REPRESENTATION_CONTEXT ( 3 ) GLOBAL_UNCERTAINTY_ASSIGNED_CONTEXT ( ( #1462 ) ) GLOBAL_UNIT_ASSIGNED_CONTEXT ( ( #12067, #11284, #11162 ) ) REPRESENTATION_CONTEXT ( 'NONE', 'WORKASPACE' ) );
#4903 = CARTESIAN_POINT ( 'NONE',  ( 1.500000000000000444, -13.28910708463142498, 20.93895013827577145 ) ) ;
#4904 = CARTESIAN_POINT ( 'NONE',  ( -3.406233159845096559, 11.94786423299364486, 6.857782953271941950E-17 ) ) ;
#4905 = DIRECTION ( 'NONE',  ( 1.000000000000000000, 0.000000000000000000, 0.000000000000000000 ) ) ;
#4906 = ORIENTED_EDGE ( 'NONE', *, *, #3849, .T. ) ;
#4907 = ADVANCED_FACE ( 'NONE', ( #8390 ), #982, .T. ) ;
#4908 = DIRECTION ( 'NONE',  ( -1.000000000000000000, 0.000000000000000000, 0.000000000000000000 ) ) ;
#4909 = CARTESIAN_POINT ( 'NONE',  ( 3.000000000000000888, -22.83456483164687256, -2.745295967526231173 ) ) ;
#4910 = AXIS2_PLACEMENT_3D ( 'NONE', #8011, #7206, #8824 ) ;
#4911 = ORIENTED_EDGE ( 'NONE', *, *, #2466, .F. ) ;
#4912 = VECTOR ( 'NONE', #5802, 1000.000000000000000 ) ;
#4913 = CARTESIAN_POINT ( 'NONE',  ( -7.115032382426030644, -13.85544350050026807, 10.00000000000000000 ) ) ;
#4914 = DIRECTION ( 'NONE',  ( -1.000000000000000000, 0.000000000000000000, -0.000000000000000000 ) ) ;
#4915 = AXIS2_PLACEMENT_3D ( 'NONE', #2874, #5690, #9419 ) ;
#4917 = AXIS2_PLACEMENT_3D ( 'NONE', #3535, #6107, #9043 ) ;
#4916 = CYLINDRICAL_SURFACE ( 'NONE', #3671, 9.599999999999997868 ) ;
#4918 = AXIS2_PLACEMENT_3D ( 'NONE', #11602, #7804, #11539 ) ;
#4919 = CARTESIAN_POINT ( 'NONE',  ( 22.00000000000000000, 2.694222958124176809E-15, 3.000000000000000000 ) ) ;
#4920 = CARTESIAN_POINT ( 'NONE',  ( 11.37845468071832222, 2.456417158213071161, 10.00000000000000000 ) ) ;
#4921 = CYLINDRICAL_SURFACE ( 'NONE', #10395, 9.599999999999997868 ) ;
#4922 = CARTESIAN_POINT ( 'NONE',  ( 15.52845182490561271, -5.270724383582042094, 3.747395293195558847E-16 ) ) ;
#4923 = CARTESIAN_POINT ( 'NONE',  ( 8.000000000000000000, 0.000000000000000000, 0.000000000000000000 ) ) ;
#4924 = EDGE_LOOP ( 'NONE', ( #5696, #5611, #2722, #4488 ) ) ;
#4925 = DIRECTION ( 'NONE',  ( -1.000000000000000000, -0.000000000000000000, -0.000000000000000000 ) ) ;
#4926 = PRODUCT_DEFINITION_SHAPE ( 'NONE', 'NONE',  #8151 ) ;
#4927 = ORIENTED_EDGE ( 'NONE', *, *, #10436, .T. ) ;
#4928 = AXIS2_PLACEMENT_3D ( 'NONE', #6366, #7385, #915 ) ;
#4929 = VERTEX_POINT ( 'NONE', #10280 ) ;
#4930 = CARTESIAN_POINT ( 'NONE',  ( 0.000000000000000000, 9.128825345753341480, -23.05871956130112821 ) ) ;
#4931 = CARTESIAN_POINT ( 'NONE',  ( -6.036922680726761747, -0.4347383792561346771, 10.00000000000000000 ) ) ;
#4932 = LINE ( 'NONE', #11242, #352 ) ;
#4933 = DIRECTION ( 'NONE',  ( -1.000000000000000000, 0.000000000000000000, 0.000000000000000000 ) ) ;
#4934 = CIRCLE ( 'NONE', #9624, 3.500000000000000000 ) ;
#4935 = CARTESIAN_POINT ( 'NONE',  ( 7.763517025773944980, -3.069710483245354116, 10.00000000000000000 ) ) ;
#4936 = EDGE_CURVE ( 'NONE', #5220, #219, #653, .T. ) ;
#4937 = CARTESIAN_POINT ( 'NONE',  ( 13.06601448280974509, -5.920767845834311593, 6.857782953271941950E-17 ) ) ;
#4938 = DIRECTION ( 'NONE',  ( -1.000000000000000000, -0.000000000000000000, 0.000000000000000000 ) ) ;
#4939 = AXIS2_PLACEMENT_3D ( 'NONE', #4999, #3168, #7107 ) ;
#4940 = DIRECTION ( 'NONE',  ( -1.000000000000000000, 0.000000000000000000, 0.000000000000000000 ) ) ;
#4941 = ORIENTED_EDGE ( 'NONE', *, *, #7024, .F. ) ;
#4942 = EDGE_CURVE ( 'NONE', #9445, #10348, #1102, .T. ) ;
#4943 = EDGE_CURVE ( 'NONE', #6369, #8696, #4176, .T. ) ;
#4944 = VERTEX_POINT ( 'NONE', #8573 ) ;
#4945 = DIRECTION ( 'NONE',  ( 0.000000000000000000, 0.000000000000000000, 1.000000000000000000 ) ) ;
#4946 = AXIS2_PLACEMENT_3D ( 'NONE', #4527, #6362, #5258 ) ;
#4947 = DIRECTION ( 'NONE',  ( -1.000000000000000000, -0.000000000000000000, 0.000000000000000000 ) ) ;
#4948 = EDGE_CURVE ( 'NONE', #5148, #6070, #7641, .T. ) ;
#4949 = LINE ( 'NONE', #102, #8980 ) ;
#4950 = DIRECTION ( 'NONE',  ( 1.000000000000000000, 0.000000000000000000, 0.000000000000000000 ) ) ;
#4951 = CARTESIAN_POINT ( 'NONE',  ( 6.685168693379560878, -7.607270790100919555, 3.747395293195558847E-16 ) ) ;
#4952 = AXIS2_PLACEMENT_3D ( 'NONE', #5214, #7275, #8022 ) ;
#4953 = EDGE_CURVE ( 'NONE', #8886, #10656, #2079, .T. ) ;
#4954 = DIRECTION ( 'NONE',  ( -1.000000000000000000, 0.000000000000000000, 0.000000000000000000 ) ) ;
#4955 = ORIENTED_EDGE ( 'NONE', *, *, #619, .F. ) ;
#4956 = AXIS2_PLACEMENT_3D ( 'NONE', #4641, #11120, #7376 ) ;
#4957 = ORIENTED_EDGE ( 'NONE', *, *, #3605, .F. ) ;
#4958 = CARTESIAN_POINT ( 'NONE',  ( -10.85385039129053197, -12.37615246896657872, 10.00000000000000000 ) ) ;
#4959 = ORIENTED_EDGE ( 'NONE', *, *, #3414, .F. ) ;
#4960 = LINE ( 'NONE', #8699, #5460 ) ;
#4961 = CARTESIAN_POINT ( 'NONE',  ( 3.000000000000000888, 22.37663021667344054, -2.811977935937859385 ) ) ;
#4962 = AXIS2_PLACEMENT_3D ( 'NONE', #10390, #10328, #8508 ) ;
#4963 = LINE ( 'NONE', #3984, #1688 ) ;
#4964 = ORIENTED_EDGE ( 'NONE', *, *, #11879, .F. ) ;
#4965 = CARTESIAN_POINT ( 'NONE',  ( 3.000000000000000888, 0.000000000000000000, 0.000000000000000000 ) ) ;
#4966 = EDGE_CURVE ( 'NONE', #5082, #11972, #4895, .T. ) ;
#4967 = CARTESIAN_POINT ( 'NONE',  ( 0.000000000000000000, 11.48910920600714647, -21.97817939804027176 ) ) ;
#4968 = CARTESIAN_POINT ( 'NONE',  ( -5.414455899168758357, -12.47541146648942245, 6.857782953271941950E-17 ) ) ;
#4969 = ORIENTED_EDGE ( 'NONE', *, *, #5549, .T. ) ;
#4970 = EDGE_CURVE ( 'NONE', #4404, #2419, #2024, .T. ) ;
#4971 = CARTESIAN_POINT ( 'NONE',  ( 3.000000000000000888, 19.29833442572375546, -11.67026512804527272 ) ) ;
#4972 = AXIS2_PLACEMENT_3D ( 'NONE', #2602, #884, #12070 ) ;
#4973 = DIRECTION ( 'NONE',  ( 0.000000000000000000, 0.000000000000000000, 1.000000000000000000 ) ) ;
#4974 = ORIENTED_EDGE ( 'NONE', *, *, #10184, .F. ) ;
#4975 = CARTESIAN_POINT ( 'NONE',  ( 6.685168693379562654, -7.607270790100137958, 10.00000000000000000 ) ) ;
#4976 = LINE ( 'NONE', #8944, #6183 ) ;
#4977 = EDGE_CURVE ( 'NONE', #9866, #7518, #6781, .T. ) ;
#4978 = ORIENTED_EDGE ( 'NONE', *, *, #11157, .T. ) ;
#4979 = AXIS2_PLACEMENT_3D ( 'NONE', #1480, #9868, #5215 ) ;
#4980 = LINE ( 'NONE', #8833, #6405 ) ;
#4981 = CARTESIAN_POINT ( 'NONE',  ( 3.000000000000000888, 0.000000000000000000, 0.000000000000000000 ) ) ;
#4982 = CARTESIAN_POINT ( 'NONE',  ( -10.47176928358605075, -8.303818807687077808, 10.00000000000000000 ) ) ;
#4983 = DIRECTION ( 'NONE',  ( 0.000000000000000000, 0.000000000000000000, 1.000000000000000000 ) ) ;
#4984 = CARTESIAN_POINT ( 'NONE',  ( -13.25288834650809555, -7.646628085888695914, 3.747395293195558847E-16 ) ) ;
#4985 = CYLINDRICAL_SURFACE ( 'NONE', #9194, 9.599999999999997868 ) ;
#4986 = CARTESIAN_POINT ( 'NONE',  ( 3.000000000000000888, -3.623565124517270419, 24.53384959170456270 ) ) ;
#4987 = VERTEX_POINT ( 'NONE', #3293 ) ;
#4988 = ORIENTED_EDGE ( 'NONE', *, *, #9648, .T. ) ;
#4989 = CARTESIAN_POINT ( 'NONE',  ( 3.000000000000000888, 24.02068490260620948, -6.168200451485520652 ) ) ;
#4990 = CARTESIAN_POINT ( 'NONE',  ( 5.498207398719435091, -4.630339417915830147, 10.00000000000000000 ) ) ;
#4991 = ADVANCED_FACE ( 'NONE', ( #7761 ), #11500, .T. ) ;
#4992 = DIRECTION ( 'NONE',  ( -1.000000000000000000, 0.000000000000000000, 0.000000000000000000 ) ) ;
#4993 = CARTESIAN_POINT ( 'NONE',  ( 10.96671743108979058, -3.132869264233008266, 10.00000000000000000 ) ) ;
#4994 = CARTESIAN_POINT ( 'NONE',  ( 5.564773995946417529, -12.83798980516507626, 6.857782953271941950E-17 ) ) ;
#4995 = CYLINDRICAL_SURFACE ( 'NONE', #9995, 24.80000000000000071 ) ;
#4996 = CARTESIAN_POINT ( 'NONE',  ( 3.000000000000000888, 15.42759117534407309, -16.45023496161649845 ) ) ;
#4997 = ORIENTED_EDGE ( 'NONE', *, *, #3289, .T. ) ;
#4998 = ORIENTED_EDGE ( 'NONE', *, *, #11961, .T. ) ;
#4999 = CARTESIAN_POINT ( 'NONE',  ( 3.000000000000000888, 0.000000000000000000, 0.000000000000000000 ) ) ;
#5000 = VECTOR ( 'NONE', #7108, 1000.000000000000000 ) ;
#5001 = CYLINDRICAL_SURFACE ( 'NONE', #7450, 24.80000000000000071 ) ;
#5002 = DIRECTION ( 'NONE',  ( -0.000000000000000000, -0.000000000000000000, 1.000000000000000000 ) ) ;
#5003 = LINE ( 'NONE', #6037, #8374 ) ;
#5004 = CARTESIAN_POINT ( 'NONE',  ( -6.777230418910821896, -10.52530689671158193, 3.747395293195558847E-16 ) ) ;
#5005 = AXIS2_PLACEMENT_3D ( 'NONE', #7033, #6918, #10661 ) ;
#5006 = ADVANCED_FACE ( 'NONE', ( #6903 ), #7014, .F. ) ;
#5007 = ADVANCED_FACE ( 'NONE', ( #2199 ), #11673, .T. ) ;
#5008 = CARTESIAN_POINT ( 'NONE',  ( 3.000000000000000888, -9.589108953447752270, -20.41249101028221702 ) ) ;
#5009 = VERTEX_POINT ( 'NONE', #9778 ) ;
#5010 = VERTEX_POINT ( 'NONE', #5876 ) ;
#5011 = DIRECTION ( 'NONE',  ( 1.000000000000000000, 0.000000000000000000, 0.000000000000000000 ) ) ;
#5012 = CARTESIAN_POINT ( 'NONE',  ( 5.334478431285540445, 14.15651896542077104, 10.00000000000000000 ) ) ;
#5013 = ORIENTED_EDGE ( 'NONE', *, *, #11305, .F. ) ;
#5014 = DIRECTION ( 'NONE',  ( 0.000000000000000000, 0.000000000000000000, 1.000000000000000000 ) ) ;
#5015 = DIRECTION ( 'NONE',  ( -1.000000000000000000, -0.000000000000000000, -0.000000000000000000 ) ) ;
#5016 = CARTESIAN_POINT ( 'NONE',  ( 3.000000000000000888, -1.901833551798098876, -22.47229024614979309 ) ) ;
#5017 = AXIS2_PLACEMENT_3D ( 'NONE', #3738, #2020, #984 ) ;
#5018 = ORIENTED_EDGE ( 'NONE', *, *, #3022, .T. ) ;
#5019 = EDGE_CURVE ( 'NONE', #9635, #5247, #9720, .T. ) ;
#5020 = CARTESIAN_POINT ( 'NONE',  ( 3.000000000000000888, -4.240409074143949297, -22.15038895030653521 ) ) ;
#5021 = ADVANCED_FACE ( 'NONE', ( #1402 ), #10647, .T. ) ;
#5022 = CARTESIAN_POINT ( 'NONE',  ( 3.000000000000000888, -23.24434456306319419, -8.645255683529244450 ) ) ;
#5023 = CARTESIAN_POINT ( 'NONE',  ( 13.99323099382916169, 4.495563823643927037, 6.857782953271941950E-17 ) ) ;
#5024 = PRODUCT_DEFINITION_SHAPE ( 'NONE', 'NONE',  #9275 ) ;
#5025 = ORIENTED_EDGE ( 'NONE', *, *, #9191, .F. ) ;
#5026 = CYLINDRICAL_SURFACE ( 'NONE', #5101, 24.80000000000000071 ) ;
#5027 = DIRECTION ( 'NONE',  ( -1.000000000000000000, 0.000000000000000000, 0.000000000000000000 ) ) ;
#5028 = VERTEX_POINT ( 'NONE', #9850 ) ;
#5029 = CARTESIAN_POINT ( 'NONE',  ( -1.719633853164447057, -9.543036404944420070, 10.00000000000000000 ) ) ;
#5030 = DIRECTION ( 'NONE',  ( 0.000000000000000000, 0.000000000000000000, -1.000000000000000000 ) ) ;
#5031 =( LENGTH_UNIT ( ) NAMED_UNIT ( * ) SI_UNIT ( .MILLI., .METRE. ) );
#5032 = EDGE_CURVE ( 'NONE', #8778, #9064, #4162, .T. ) ;
#5033 = CARTESIAN_POINT ( 'NONE',  ( 0.000000000000000000, 0.000000000000000000, 0.000000000000000000 ) ) ;
#5034 = DIRECTION ( 'NONE',  ( -1.000000000000000000, 0.000000000000000000, 0.000000000000000000 ) ) ;
#5035 = CARTESIAN_POINT ( 'NONE',  ( -8.211874628637442441, -10.69266484962706620, 10.00000000000000000 ) ) ;
#5036 = AXIS2_PLACEMENT_3D ( 'NONE', #11948, #8287, #12013 ) ;
#5037 =( NAMED_UNIT ( * ) SI_UNIT ( $, .STERADIAN. ) SOLID_ANGLE_UNIT ( ) );
#5038 = CARTESIAN_POINT ( 'NONE',  ( 7.795318149608630343, -14.02504990431079612, 3.747395293195558847E-16 ) ) ;
#5039 = LINE ( 'NONE', #2047, #3534 ) ;
#5040 = ORIENTED_EDGE ( 'NONE', *, *, #1149, .F. ) ;
#5041 = CARTESIAN_POINT ( 'NONE',  ( 3.000000000000000888, 22.54798042742718067, -0.4575788569252652871 ) ) ;
#5042 = VERTEX_POINT ( 'NONE', #6117 ) ;
#5043 = VERTEX_POINT ( 'NONE', #2259 ) ;
#5044 = AXIS2_PLACEMENT_3D ( 'NONE', #2336, #6138, #8657 ) ;
#5045 = CARTESIAN_POINT ( 'NONE',  ( 0.000000000000000000, 22.42251312757879234, 5.117118920208566735 ) ) ;
#5046 = EDGE_CURVE ( 'NONE', #3562, #11246, #9061, .T. ) ;
#5047 = DIRECTION ( 'NONE',  ( 0.000000000000000000, 0.000000000000000000, 1.000000000000000000 ) ) ;
#5048 = CARTESIAN_POINT ( 'NONE',  ( -7.708066421255711731, 5.920849505456871498, 10.00000000000000000 ) ) ;
#5049 = CARTESIAN_POINT ( 'NONE',  ( 5.334478431285537781, 14.15651896542076749, 6.857782953271941950E-17 ) ) ;
#5050 = CARTESIAN_POINT ( 'NONE',  ( 3.000000000000000888, -21.97702544527753332, -6.779701584702958250 ) ) ;
#5051 = DIRECTION ( 'NONE',  ( -1.000000000000000000, 0.000000000000000000, 0.000000000000000000 ) ) ;
#5052 = ORIENTED_EDGE ( 'NONE', *, *, #2759, .T. ) ;
#5053 = EDGE_CURVE ( 'NONE', #5601, #10654, #5195, .T. ) ;
#5054 = ORIENTED_EDGE ( 'NONE', *, *, #1964, .T. ) ;
#5055 = VERTEX_POINT ( 'NONE', #8700 ) ;
#5056 = FACE_OUTER_BOUND ( 'NONE', #9131, .T. ) ;
#5057 = DIRECTION ( 'NONE',  ( -1.000000000000000000, -0.000000000000000000, -0.000000000000000000 ) ) ;
#5058 = CIRCLE ( 'NONE', #10138, 24.80000000000000071 ) ;
#5059 = PRESENTATION_STYLE_ASSIGNMENT (( #3416 ) ) ;
#5060 = DIRECTION ( 'NONE',  ( 1.000000000000000000, -0.000000000000000000, -0.000000000000000000 ) ) ;
#5061 = AXIS2_PLACEMENT_3D ( 'NONE', #1078, #4809, #1493 ) ;
#5062 = CARTESIAN_POINT ( 'NONE',  ( 10.41236255589546822, -1.188820951657898473, 3.747395293195558847E-16 ) ) ;
#5063 = CARTESIAN_POINT ( 'NONE',  ( 3.000000000000000888, -17.06259499759935139, -14.74749645580028101 ) ) ;
#5064 =( GEOMETRIC_REPRESENTATION_CONTEXT ( 3 ) GLOBAL_UNCERTAINTY_ASSIGNED_CONTEXT ( ( #1826 ) ) GLOBAL_UNIT_ASSIGNED_CONTEXT ( ( #3721, #1825, #5499 ) ) REPRESENTATION_CONTEXT ( 'NONE', 'WORKASPACE' ) );
#5065 = VERTEX_POINT ( 'NONE', #3121 ) ;
#5066 = ORIENTED_EDGE ( 'NONE', *, *, #1061, .F. ) ;
#5067 = CARTESIAN_POINT ( 'NONE',  ( -11.39998097177319636, 5.856612080558658562, 10.00000000000000000 ) ) ;
#5068 = VERTEX_POINT ( 'NONE', #1460 ) ;
#5069 = CARTESIAN_POINT ( 'NONE',  ( 3.000000000000000888, 9.667200211209818761, 20.86861857134737264 ) ) ;
#5070 = DIRECTION ( 'NONE',  ( -1.000000000000000000, 0.000000000000000000, 0.000000000000000000 ) ) ;
#5071 = CARTESIAN_POINT ( 'NONE',  ( 0.000000000000000000, -6.779701584702887196, 21.97702544527755464 ) ) ;
#5072 = VERTEX_POINT ( 'NONE', #296 ) ;
#5073 = DIRECTION ( 'NONE',  ( -1.000000000000000000, -0.000000000000000000, 0.000000000000000000 ) ) ;
#5074 = CIRCLE ( 'NONE', #4692, 9.599999999999997868 ) ;
#5075 = DIRECTION ( 'NONE',  ( 0.000000000000000000, 0.9781476007338062439, -0.2079116908177564282 ) ) ;
#5076 = CARTESIAN_POINT ( 'NONE',  ( -10.03906249502028558, -0.8181230654450031281, 6.857782953271941950E-17 ) ) ;
#5077 = ORIENTED_EDGE ( 'NONE', *, *, #11554, .T. ) ;
#5078 = DIRECTION ( 'NONE',  ( -1.000000000000000000, 0.000000000000000000, 0.000000000000000000 ) ) ;
#5079 = EDGE_LOOP ( 'NONE', ( #1332, #5947, #10444, #618 ) ) ;
#5080 = FACE_OUTER_BOUND ( 'NONE', #421, .T. ) ;
#5081 = AXIS2_PLACEMENT_3D ( 'NONE', #11540, #4076, #10626 ) ;
#5082 = VERTEX_POINT ( 'NONE', #4033 ) ;
#5083 = EDGE_CURVE ( 'NONE', #10038, #8212, #1634, .T. ) ;
#5084 = CARTESIAN_POINT ( 'NONE',  ( -8.457858257355617582, -3.686763380685291747, 10.00000000000000000 ) ) ;
#5085 = ADVANCED_FACE ( 'NONE', ( #11620 ), #8001, .T. ) ;
#5086 = CIRCLE ( 'NONE', #11721, 9.599999999999997868 ) ;
#5087 = ORIENTED_EDGE ( 'NONE', *, *, #11480, .F. ) ;
#5088 = DIRECTION ( 'NONE',  ( 0.000000000000000000, 0.000000000000000000, 1.000000000000000000 ) ) ;
#5089 = CARTESIAN_POINT ( 'NONE',  ( 0.000000000000000000, -21.14796121233203152, 9.039786367038763260 ) ) ;
#5090 = DIRECTION ( 'NONE',  ( -1.000000000000000000, -0.000000000000000000, -0.000000000000000000 ) ) ;
#5091 = CARTESIAN_POINT ( 'NONE',  ( -9.960937504979712642, 0.8181230654450121209, 10.00000000000000000 ) ) ;
#5092 = AXIS2_PLACEMENT_3D ( 'NONE', #7855, #5962, #1125 ) ;
#5093 = DIRECTION ( 'NONE',  ( 0.000000000000000000, 0.000000000000000000, 1.000000000000000000 ) ) ;
#5094 = AXIS2_PLACEMENT_3D ( 'NONE', #725, #3493, #4461 ) ;
#5095 = CARTESIAN_POINT ( 'NONE',  ( -11.08238827499517321, -10.71925978067678642, 3.747395293195558847E-16 ) ) ;
#5096 = CIRCLE ( 'NONE', #4511, 9.599999999999997868 ) ;
#5097 = DIRECTION ( 'NONE',  ( 0.000000000000000000, 0.000000000000000000, 1.000000000000000000 ) ) ;
#5098 =( GEOMETRIC_REPRESENTATION_CONTEXT ( 3 ) GLOBAL_UNCERTAINTY_ASSIGNED_CONTEXT ( ( #7945 ) ) GLOBAL_UNIT_ASSIGNED_CONTEXT ( ( #374, #9801, #7779 ) ) REPRESENTATION_CONTEXT ( 'NONE', 'WORKASPACE' ) );
#5099 = CARTESIAN_POINT ( 'NONE',  ( 0.000000000000000000, -18.51065745848386968, 12.88318129270172818 ) ) ;
#5100 = ORIENTED_EDGE ( 'NONE', *, *, #10281, .T. ) ;
#5101 = AXIS2_PLACEMENT_3D ( 'NONE', #4045, #4103, #1234 ) ;
#5102 = AXIS2_PLACEMENT_3D ( 'NONE', #2369, #11725, #9953 ) ;
#5103 = DIRECTION ( 'NONE',  ( 0.000000000000000000, 0.000000000000000000, 1.000000000000000000 ) ) ;
#5104 = CYLINDRICAL_SURFACE ( 'NONE', #140, 9.599999999999997868 ) ;
#5105 = CARTESIAN_POINT ( 'NONE',  ( 0.000000000000000000, 1.556492618230966851, -24.75110766671650708 ) ) ;
#5106 = CARTESIAN_POINT ( 'NONE',  ( -0.1504880127287666625, 9.287785325659767111, 10.00000000000000000 ) ) ;
#5107 = EDGE_CURVE ( 'NONE', #4686, #5213, #4481, .T. ) ;
#5108 = CARTESIAN_POINT ( 'NONE',  ( 11.40744677810890373, -1.317628706759688129, 6.857782953271941950E-17 ) ) ;
#5109 = CARTESIAN_POINT ( 'NONE',  ( 3.000000000000000888, 21.76479567747241717, 7.432877647175279101 ) ) ;
#5110 = CIRCLE ( 'NONE', #6671, 9.599999999999996092 ) ;
#5111 = DIRECTION ( 'NONE',  ( 1.000000000000000000, 0.000000000000000000, 0.000000000000000000 ) ) ;
#5112 = VECTOR ( 'NONE', #7614, 1000.000000000000000 ) ;
#5113 = EDGE_LOOP ( 'NONE', ( #1854, #3603, #890, #7593 ) ) ;
#5114 = CIRCLE ( 'NONE', #9806, 9.599999999999999645 ) ;
#5115 = ADVANCED_FACE ( 'NONE', ( #354 ), #4095, .T. ) ;
#5116 = ORIENTED_EDGE ( 'NONE', *, *, #7174, .F. ) ;
#5117 = ORIENTED_EDGE ( 'NONE', *, *, #3849, .F. ) ;
#5118 = ADVANCED_FACE ( 'NONE', ( #4215, #11978 ), #4518, .T. ) ;
#5119 = CARTESIAN_POINT ( 'NONE',  ( 0.000000000000000000, 11.20082935824075321, 20.08719549084868561 ) ) ;
#5120 = AXIS2_PLACEMENT_3D ( 'NONE', #4799, #11520, #10426 ) ;
#5121 = DIRECTION ( 'NONE',  ( 1.000000000000000000, 0.000000000000000000, 0.000000000000000000 ) ) ;
#5122 = CARTESIAN_POINT ( 'NONE',  ( 0.000000000000000000, -19.75591328264893676, 10.87771529938155268 ) ) ;
#5123 = ADVANCED_FACE ( 'NONE', ( #3486 ), #5496, .T. ) ;
#5124 = APPLICATION_CONTEXT ( 'automotive_design' ) ;
#5125 = CARTESIAN_POINT ( 'NONE',  ( -8.799590028668786701, 7.703979956834778875, 3.747395293195558847E-16 ) ) ;
#5126 = CARTESIAN_POINT ( 'NONE',  ( 1.499999999999999556, 24.53384959170457336, 3.623565124517186931 ) ) ;
#5127 = SHAPE_REPRESENTATION ( 'housing', ( #8474 ), #5529 ) ;
#5128 = DIRECTION ( 'NONE',  ( 0.000000000000000000, 0.000000000000000000, 1.000000000000000000 ) ) ;
#5129 = ORIENTED_EDGE ( 'NONE', *, *, #2630, .F. ) ;
#5130 = ORIENTED_EDGE ( 'NONE', *, *, #819, .T. ) ;
#5131 = CONTEXT_DEPENDENT_SHAPE_REPRESENTATION ( #7378, #9314 ) ;
#5132 = CARTESIAN_POINT ( 'NONE',  ( 14.53830338343600559, -0.2437330612273629071, 10.00000000000000000 ) ) ;
#5133 = ORIENTED_EDGE ( 'NONE', *, *, #1938, .F. ) ;
#5134 = CARTESIAN_POINT ( 'NONE',  ( 0.000000000000000000, -19.75591328264879110, -10.87771529938182091 ) ) ;
#5135 = CARTESIAN_POINT ( 'NONE',  ( 1.499999999999999556, 11.02759168516744737, 22.21333432029567589 ) ) ;
#5136 = CARTESIAN_POINT ( 'NONE',  ( 3.000000000000000888, -12.88318129270165890, -18.51065745848391586 ) ) ;
#5137 = EDGE_LOOP ( 'NONE', ( #7914, #2375, #9691, #4141 ) ) ;
#5138 = CIRCLE ( 'NONE', #8670, 9.599999999999999645 ) ;
#5139 = CARTESIAN_POINT ( 'NONE',  ( 3.000000000000000888, 0.000000000000000000, 0.000000000000000000 ) ) ;
#5140 = DIRECTION ( 'NONE',  ( 0.000000000000000000, 0.000000000000000000, 1.000000000000000000 ) ) ;
#5141 = CARTESIAN_POINT ( 'NONE',  ( 8.143984375791809782, 3.063465613658396425, 6.857782953271941950E-17 ) ) ;
#5142 = CIRCLE ( 'NONE', #1822, 22.99899999999999878 ) ;
#5143 = CIRCLE ( 'NONE', #3396, 9.599999999999996092 ) ;
#5144 = ORIENTED_EDGE ( 'NONE', *, *, #3070, .T. ) ;
#5145 = DIRECTION ( 'NONE',  ( 0.000000000000000000, 0.000000000000000000, 1.000000000000000000 ) ) ;
#5146 = ORIENTED_EDGE ( 'NONE', *, *, #5486, .F. ) ;
#5147 = DIRECTION ( 'NONE',  ( -1.000000000000000000, -0.000000000000000000, -0.000000000000000000 ) ) ;
#5148 = VERTEX_POINT ( 'NONE', #779 ) ;
#5149 = CARTESIAN_POINT ( 'NONE',  ( -8.799590028668788477, 7.703979956833879150, 10.00000000000000000 ) ) ;
#5150 = DIRECTION ( 'NONE',  ( 0.000000000000000000, 0.000000000000000000, -1.000000000000000000 ) ) ;
#5151 = VERTEX_POINT ( 'NONE', #6178 ) ;
#5152 = CARTESIAN_POINT ( 'NONE',  ( 3.000000000000000888, 0.4575788569254873317, -22.54798042742717712 ) ) ;
#5153 = DIRECTION ( 'NONE',  ( 0.000000000000000000, -1.000000000000000000, -1.048062100069321321E-14 ) ) ;
#5154 = CARTESIAN_POINT ( 'NONE',  ( 9.246005348854476225, -6.405614325510554430, 10.00000000000000000 ) ) ;
#5155 = AXIS2_PLACEMENT_3D ( 'NONE', #8289, #4373, #4431 ) ;
#5156 = DIRECTION ( 'NONE',  ( -1.000000000000000000, 0.000000000000000000, 0.000000000000000000 ) ) ;
#5157 = CARTESIAN_POINT ( 'NONE',  ( -10.73274959028096198, -5.974010873319483217, 3.747395293195558847E-16 ) ) ;
#5158 = EDGE_CURVE ( 'NONE', #505, #3056, #8253, .T. ) ;
#5159 = CYLINDRICAL_SURFACE ( 'NONE', #2356, 9.599999999999997868 ) ;
#5160 = EDGE_CURVE ( 'NONE', #5042, #5965, #2728, .T. ) ;
#5161 = EDGE_CURVE ( 'NONE', #5009, #8199, #11128, .T. ) ;
#5162 = CYLINDRICAL_SURFACE ( 'NONE', #2162, 9.599999999999997868 ) ;
#5163 = ORIENTED_EDGE ( 'NONE', *, *, #819, .F. ) ;
#5164 = CIRCLE ( 'NONE', #475, 9.599999999999996092 ) ;
#5165 = DIRECTION ( 'NONE',  ( -1.000000000000000000, 0.000000000000000000, -0.000000000000000000 ) ) ;
#5166 = ORIENTED_EDGE ( 'NONE', *, *, #2693, .T. ) ;
#5167 = CYLINDRICAL_SURFACE ( 'NONE', #7569, 9.599999999999997868 ) ;
#5168 = VERTEX_POINT ( 'NONE', #10887 ) ;
#5169 = CYLINDRICAL_SURFACE ( 'NONE', #3412, 9.599999999999997868 ) ;
#5170 = CARTESIAN_POINT ( 'NONE',  ( -5.924299593718521884, 3.297400215539481039, 10.00000000000000000 ) ) ;
#5171 = ADVANCED_FACE ( 'NONE', ( #2677 ), #4396, .T. ) ;
#5172 = CARTESIAN_POINT ( 'NONE',  ( -7.708066421255707290, 5.920849505456867945, 6.857782953271941950E-17 ) ) ;
#5173 = LINE ( 'NONE', #1498, #7653 ) ;
#5174 = EDGE_CURVE ( 'NONE', #8841, #6834, #3307, .T. ) ;
#5175 = CIRCLE ( 'NONE', #10845, 9.599999999999997868 ) ;
#5176 = DIRECTION ( 'NONE',  ( -1.000000000000000000, 0.000000000000000000, 0.000000000000000000 ) ) ;
#5177 = ORIENTED_EDGE ( 'NONE', *, *, #7333, .T. ) ;
#5178 = ORIENTED_EDGE ( 'NONE', *, *, #8312, .F. ) ;
#5179 = VERTEX_POINT ( 'NONE', #9231 ) ;
#5180 = EDGE_CURVE ( 'NONE', #10578, #8389, #3124, .T. ) ;
#5181 = CARTESIAN_POINT ( 'NONE',  ( 12.15471013770155295, -5.500887282572486825, 10.00000000000000000 ) ) ;
#5182 = SURFACE_STYLE_FILL_AREA ( #1447 ) ;
#5183 = DIRECTION ( 'NONE',  ( -1.000000000000000000, 0.000000000000000000, 0.000000000000000000 ) ) ;
#5184 = EDGE_CURVE ( 'NONE', #10794, #2327, #2138, .T. ) ;
#5185 = CARTESIAN_POINT ( 'NONE',  ( 4.140589500486089314, -5.731468560950439439, 3.747395293195558847E-16 ) ) ;
#5186 = DIRECTION ( 'NONE',  ( 0.000000000000000000, 0.000000000000000000, 1.000000000000000000 ) ) ;
#5187 = DIRECTION ( 'NONE',  ( 0.000000000000000000, 0.000000000000000000, -1.000000000000000000 ) ) ;
#5188 = ORIENTED_EDGE ( 'NONE', *, *, #6513, .F. ) ;
#5189 = ORIENTED_EDGE ( 'NONE', *, *, #11625, .F. ) ;
#5190 = AXIS2_PLACEMENT_3D ( 'NONE', #9444, #5777, #187 ) ;
#5191 = CARTESIAN_POINT ( 'NONE',  ( -8.211874628637442441, -10.69266484962706620, 10.00000000000000000 ) ) ;
#5192 = VERTEX_POINT ( 'NONE', #7075 ) ;
#5193 = CARTESIAN_POINT ( 'NONE',  ( 1.631735293711821022, 4.895207720155140940, 10.00000000000000000 ) ) ;
#5194 = CARTESIAN_POINT ( 'NONE',  ( -10.00000000000000000, 0.000000000000000000, 0.000000000000000000 ) ) ;
#5195 = LINE ( 'NONE', #2315, #8077 ) ;
#5196 = CARTESIAN_POINT ( 'NONE',  ( 3.000000000000000888, 0.000000000000000000, 0.000000000000000000 ) ) ;
#5197 = EDGE_LOOP ( 'NONE', ( #10913, #9560, #112, #977 ) ) ;
#5198 = EDGE_CURVE ( 'NONE', #3033, #7795, #11522, .T. ) ;
#5199 = DIRECTION ( 'NONE',  ( -1.000000000000000000, -0.000000000000000000, 0.000000000000000000 ) ) ;
#5200 = AXIS2_PLACEMENT_3D ( 'NONE', #1775, #1713, #9918 ) ;
#5201 = CYLINDRICAL_SURFACE ( 'NONE', #7464, 9.599999999999997868 ) ;
#5202 = CARTESIAN_POINT ( 'NONE',  ( -8.665663522307772482, -5.581295667939712324, 6.857782953271941950E-17 ) ) ;
#5203 = EDGE_LOOP ( 'NONE', ( #10957, #5950, #978, #350 ) ) ;
#5204 = CYLINDRICAL_SURFACE ( 'NONE', #6843, 9.599999999999997868 ) ;
#5205 = DIRECTION ( 'NONE',  ( 1.000000000000000000, 0.000000000000000000, 0.000000000000000000 ) ) ;
#5206 = EDGE_CURVE ( 'NONE', #8295, #5263, #5254, .T. ) ;
#5207 = ORIENTED_EDGE ( 'NONE', *, *, #3523, .T. ) ;
#5208 = AXIS2_PLACEMENT_3D ( 'NONE', #6118, #9853, #4898 ) ;
#5209 = CARTESIAN_POINT ( 'NONE',  ( -9.680665087126289592, -7.686621967951973389, 10.00000000000000000 ) ) ;
#5210 = ORIENTED_EDGE ( 'NONE', *, *, #10767, .T. ) ;
#5211 = LINE ( 'NONE', #8712, #8333 ) ;
#5212 = SURFACE_STYLE_FILL_AREA ( #621 ) ;
#5213 = VERTEX_POINT ( 'NONE', #1700 ) ;
#5214 = CARTESIAN_POINT ( 'NONE',  ( 3.000000000000000888, 21.58580335785685378, -6.532525787310757615 ) ) ;
#5215 = DIRECTION ( 'NONE',  ( 0.000000000000000000, 0.000000000000000000, 1.000000000000000000 ) ) ;
#5216 = CARTESIAN_POINT ( 'NONE',  ( -8.209791827104817585, -6.297951179201753291, 10.00000000000000000 ) ) ;
#5217 = CARTESIAN_POINT ( 'NONE',  ( 0.000000000000000000, 0.000000000000000000, 0.000000000000000000 ) ) ;
#5218 = CARTESIAN_POINT ( 'NONE',  ( 9.623054350189519823, -9.012277985855606133, 3.747395293195558847E-16 ) ) ;
#5219 = FACE_OUTER_BOUND ( 'NONE', #9812, .T. ) ;
#5220 = VERTEX_POINT ( 'NONE', #5320 ) ;
#5221 = CARTESIAN_POINT ( 'NONE',  ( 0.000000000000000000, -17.06259499759954679, 14.74749645580005364 ) ) ;
#5222 = ORIENTED_EDGE ( 'NONE', *, *, #11043, .T. ) ;
#5223 = CARTESIAN_POINT ( 'NONE',  ( 3.000000000000000888, 9.589108953448178596, -20.41249101028201451 ) ) ;
#5224 = ORIENTED_EDGE ( 'NONE', *, *, #3908, .F. ) ;
#5225 = CARTESIAN_POINT ( 'NONE',  ( 3.000000000000000888, -4.240409074144249502, 22.15038895030647836 ) ) ;
#5226 = EDGE_CURVE ( 'NONE', #9316, #8647, #7257, .T. ) ;
#5227 = CARTESIAN_POINT ( 'NONE',  ( -2.958039891549808953, -0.4999999999999997780, 0.000000000000000000 ) ) ;
#5228 = CARTESIAN_POINT ( 'NONE',  ( 0.000000000000000000, 4.135161237383914390, -24.45282072769597193 ) ) ;
#5229 = CARTESIAN_POINT ( 'NONE',  ( -9.820986981721938847, 1.626514086989861108, 6.857782953271941950E-17 ) ) ;
#5230 = CARTESIAN_POINT ( 'NONE',  ( 0.000000000000000000, -4.445336973060693531, -22.56530478845653676 ) ) ;
#5231 = DIRECTION ( 'NONE',  ( 0.000000000000000000, 0.000000000000000000, 1.000000000000000000 ) ) ;
#5232 = EDGE_CURVE ( 'NONE', #2526, #6927, #8977, .T. ) ;
#5233 = CIRCLE ( 'NONE', #9530, 22.00000000000000000 ) ;
#5234 = ORIENTED_EDGE ( 'NONE', *, *, #7915, .F. ) ;
#5235 = AXIS2_PLACEMENT_3D ( 'NONE', #8891, #4234, #7959 ) ;
#5236 = VERTEX_POINT ( 'NONE', #849 ) ;
#5237 = EDGE_CURVE ( 'NONE', #4165, #3870, #5432, .T. ) ;
#5238 = CARTESIAN_POINT ( 'NONE',  ( -6.777230418910823673, -10.52530689671158548, 10.00000000000000000 ) ) ;
#5239 = EDGE_CURVE ( 'NONE', #5976, #384, #5266, .T. ) ;
#5240 = DIRECTION ( 'NONE',  ( -1.000000000000000000, -0.000000000000000000, -0.000000000000000000 ) ) ;
#5241 = EDGE_CURVE ( 'NONE', #8808, #6916, #10146, .T. ) ;
#5242 = AXIS2_PLACEMENT_3D ( 'NONE', #8740, #4083, #2247 ) ;
#5243 = CARTESIAN_POINT ( 'NONE',  ( -5.962113107391269651, -1.426310550302858582, 3.747395293195558847E-16 ) ) ;
#5244 = DIRECTION ( 'NONE',  ( -1.000000000000000000, 0.000000000000000000, 0.000000000000000000 ) ) ;
#5245 = DIRECTION ( 'NONE',  ( 0.000000000000000000, 0.3090169943749417336, 0.9510565162951555296 ) ) ;
#5246 = EDGE_LOOP ( 'NONE', ( #8461, #9103, #4655, #5297 ) ) ;
#5247 = VERTEX_POINT ( 'NONE', #11799 ) ;
#5248 = CARTESIAN_POINT ( 'NONE',  ( 1.124919223378051392, -13.78906249641292270, 10.00000000000000000 ) ) ;
#5249 = ORIENTED_EDGE ( 'NONE', *, *, #5206, .T. ) ;
#5250 = CARTESIAN_POINT ( 'NONE',  ( 3.000000000000000888, 0.000000000000000000, 0.000000000000000000 ) ) ;
#5251 = AXIS2_PLACEMENT_3D ( 'NONE', #1448, #7064, #9950 ) ;
#5252 = VECTOR ( 'NONE', #1994, 1000.000000000000000 ) ;
#5253 = CARTESIAN_POINT ( 'NONE',  ( 0.000000000000000000, 0.000000000000000000, 0.000000000000000000 ) ) ;
#5254 = LINE ( 'NONE', #1756, #3707 ) ;
#5255 = DIRECTION ( 'NONE',  ( -1.000000000000000000, -0.000000000000000000, -0.000000000000000000 ) ) ;
#5256 = ORIENTED_EDGE ( 'NONE', *, *, #6870, .T. ) ;
#5257 = DIRECTION ( 'NONE',  ( -1.000000000000000000, 0.000000000000000000, 0.000000000000000000 ) ) ;
#5258 = DIRECTION ( 'NONE',  ( 0.000000000000000000, -0.9135454576425964257, -0.4067366430758102558 ) ) ;
#5259 = CARTESIAN_POINT ( 'NONE',  ( 9.246005348854470896, -6.405614325511344909, 6.857782953271941950E-17 ) ) ;
#5260 = CIRCLE ( 'NONE', #371, 9.599999999999999645 ) ;
#5261 = CARTESIAN_POINT ( 'NONE',  ( 3.000000000000000888, 22.37663021667344054, -2.811977935937859385 ) ) ;
#5262 = DIRECTION ( 'NONE',  ( 0.000000000000000000, -0.1045284632676401482, -0.9945218953682747332 ) ) ;
#5263 = VERTEX_POINT ( 'NONE', #9051 ) ;
#5264 = EDGE_CURVE ( 'NONE', #9796, #10367, #9377, .T. ) ;
#5265 = CARTESIAN_POINT ( 'NONE',  ( -2.196651480121881050, 8.111327970581173830, 10.00000000000000000 ) ) ;
#5266 = CIRCLE ( 'NONE', #2535, 9.599999999999997868 ) ;
#5267 = CIRCLE ( 'NONE', #972, 5.000000000000000000 ) ;
#5268 = VERTEX_POINT ( 'NONE', #11122 ) ;
#5269 = DIRECTION ( 'NONE',  ( -1.000000000000000000, 0.000000000000000000, 0.000000000000000000 ) ) ;
#5270 = DIRECTION ( 'NONE',  ( 1.000000000000000000, -0.000000000000000000, 0.000000000000000000 ) ) ;
#5271 = VERTEX_POINT ( 'NONE', #4642 ) ;
#5272 = VECTOR ( 'NONE', #6170, 1000.000000000000000 ) ;
#5273 = FACE_OUTER_BOUND ( 'NONE', #8160, .T. ) ;
#5274 = EDGE_CURVE ( 'NONE', #7806, #9081, #11902, .T. ) ;
#5275 = DIRECTION ( 'NONE',  ( 0.000000000000000000, 0.000000000000000000, 1.000000000000000000 ) ) ;
#5276 = CARTESIAN_POINT ( 'NONE',  ( -10.03906249502029091, -0.8181230654450249995, 10.00000000000000000 ) ) ;
#5277 = CYLINDRICAL_SURFACE ( 'NONE', #226, 9.599999999999997868 ) ;
#5278 = CARTESIAN_POINT ( 'NONE',  ( 10.36190401370965475, -8.216093097539266310, 3.747395293195558847E-16 ) ) ;
#5279 = DIRECTION ( 'NONE',  ( -1.000000000000000000, 0.000000000000000000, 0.000000000000000000 ) ) ;
#5280 = ORIENTED_EDGE ( 'NONE', *, *, #8252, .F. ) ;
#5281 = DIRECTION ( 'NONE',  ( -1.000000000000000000, 0.000000000000000000, 0.000000000000000000 ) ) ;
#5282 = CIRCLE ( 'NONE', #6270, 9.600000000000001421 ) ;
#5283 = ORIENTED_EDGE ( 'NONE', *, *, #9981, .F. ) ;
#5284 = PLANE ( 'NONE',  #2887 ) ;
#5285 = FACE_OUTER_BOUND ( 'NONE', #11987, .T. ) ;
#5286 =( LENGTH_UNIT ( ) NAMED_UNIT ( * ) SI_UNIT ( .MILLI., .METRE. ) );
#5287 = ORIENTED_EDGE ( 'NONE', *, *, #2546, .F. ) ;
#5288 = AXIS2_PLACEMENT_3D ( 'NONE', #5598, #1922, #5727 ) ;
#5289 = CARTESIAN_POINT ( 'NONE',  ( 3.000000000000000888, 23.88662356770124973, -6.668524164681381095 ) ) ;
#5290 = CIRCLE ( 'NONE', #11544, 9.599999999999997868 ) ;
#5291 = CARTESIAN_POINT ( 'NONE',  ( 3.000000000000000888, -19.10918332567968747, 15.80756504416684649 ) ) ;
#5292 = CARTESIAN_POINT ( 'NONE',  ( -4.006926059189011902, 5.225193401749456790, 10.00000000000000000 ) ) ;
#5293 = CARTESIAN_POINT ( 'NONE',  ( -8.201440678127905670, 5.289679325232165219, 6.857782953271941950E-17 ) ) ;
#5294 = PRODUCT_DEFINITION_FORMATION_WITH_SPECIFIED_SOURCE ( 'ANY', '', #11573, .NOT_KNOWN. ) ;
#5295 = DIRECTION ( 'NONE',  ( 0.000000000000000000, 0.000000000000000000, 1.000000000000000000 ) ) ;
#5296 = FACE_OUTER_BOUND ( 'NONE', #1346, .T. ) ;
#5297 = ORIENTED_EDGE ( 'NONE', *, *, #10780, .T. ) ;
#5298 = AXIS2_PLACEMENT_3D ( 'NONE', #6437, #3749, #4667 ) ;
#5299 = ORIENTED_EDGE ( 'NONE', *, *, #145, .T. ) ;
#5300 = AXIS2_PLACEMENT_3D ( 'NONE', #5427, #529, #8976 ) ;
#5301 = AXIS2_PLACEMENT_3D ( 'NONE', #9065, #547, #5262 ) ;
#5302 = EDGE_LOOP ( 'NONE', ( #5975, #2935, #8845, #2051 ) ) ;
#5303 = CARTESIAN_POINT ( 'NONE',  ( -11.74902089294173813, -3.156991809147611683, 10.00000000000000000 ) ) ;
#5304 = FACE_OUTER_BOUND ( 'NONE', #4447, .T. ) ;
#5305 = DIRECTION ( 'NONE',  ( 0.000000000000000000, 0.000000000000000000, 1.000000000000000000 ) ) ;
#5306 = AXIS2_PLACEMENT_3D ( 'NONE', #3775, #1810, #1118 ) ;
#5307 = AXIS2_PLACEMENT_3D ( 'NONE', #2983, #7686, #11424 ) ;
#5308 = VECTOR ( 'NONE', #2937, 1000.000000000000000 ) ;
#5309 = CARTESIAN_POINT ( 'NONE',  ( 2.581500635392914411, -6.456130005640034142, 3.747395293195558847E-16 ) ) ;
#5310 = AXIS2_PLACEMENT_3D ( 'NONE', #2299, #217, #1268 ) ;
#5311 = DIRECTION ( 'NONE',  ( -1.000000000000000000, 0.000000000000000000, -0.000000000000000000 ) ) ;
#5312 = EDGE_CURVE ( 'NONE', #2975, #8970, #3897, .T. ) ;
#5313 = CARTESIAN_POINT ( 'NONE',  ( 0.000000000000000000, 4.240409074144097623, 22.15038895030650679 ) ) ;
#5314 = ORIENTED_EDGE ( 'NONE', *, *, #4648, .F. ) ;
#5315 = VERTEX_POINT ( 'NONE', #5678 ) ;
#5316 = ADVANCED_FACE ( 'NONE', ( #1088, #11307 ), #10446, .T. ) ;
#5317 = CIRCLE ( 'NONE', #7253, 9.599999999999997868 ) ;
#5318 = ORIENTED_EDGE ( 'NONE', *, *, #556, .T. ) ;
#5319 = CARTESIAN_POINT ( 'NONE',  ( 3.571029491936648093, 3.388293644658559423, 10.00000000000000000 ) ) ;
#5320 = CARTESIAN_POINT ( 'NONE',  ( 3.000000000000000888, 13.79477846460820700, -18.40266524480574972 ) ) ;
#5321 = AXIS2_PLACEMENT_3D ( 'NONE', #11509, #3130, #3865 ) ;
#5322 = DIRECTION ( 'NONE',  ( -1.000000000000000000, -0.000000000000000000, 0.000000000000000000 ) ) ;
#5323 = ORIENTED_EDGE ( 'NONE', *, *, #1865, .T. ) ;
#5324 = CARTESIAN_POINT ( 'NONE',  ( 0.000000000000000000, -13.23915371906968375, 18.80635025205165434 ) ) ;
#5325 = CARTESIAN_POINT ( 'NONE',  ( 3.000000000000000888, -6.532525787310825116, -21.58580335785683246 ) ) ;
#5326 = CARTESIAN_POINT ( 'NONE',  ( -9.023584016175915323, 3.917288190900554579, 6.857782953271941950E-17 ) ) ;
#5327 = CIRCLE ( 'NONE', #8053, 9.599999999999997868 ) ;
#5328 = EDGE_CURVE ( 'NONE', #3995, #2252, #8203, .T. ) ;
#5329 = CIRCLE ( 'NONE', #10207, 24.80000000000000071 ) ;
#5330 = CIRCLE ( 'NONE', #11770, 22.99900000000000233 ) ;
#5331 = CARTESIAN_POINT ( 'NONE',  ( 3.000000000000000888, 0.000000000000000000, 0.000000000000000000 ) ) ;
#5332 = ORIENTED_EDGE ( 'NONE', *, *, #5226, .T. ) ;
#5333 = CYLINDRICAL_SURFACE ( 'NONE', #4722, 9.599999999999997868 ) ;
#5334 = EDGE_LOOP ( 'NONE', ( #9303, #7309, #2442, #11266 ) ) ;
#5335 = ORIENTED_EDGE ( 'NONE', *, *, #3756, .T. ) ;
#5336 = CARTESIAN_POINT ( 'NONE',  ( 1.831757423467613277, 7.960349185506228942, 10.00000000000000000 ) ) ;
#5337 = AXIS2_PLACEMENT_3D ( 'NONE', #9058, #3611, #3434 ) ;
#5338 = EDGE_CURVE ( 'NONE', #2284, #490, #5665, .T. ) ;
#5339 = DIRECTION ( 'NONE',  ( 4.336808689942017736E-17, 6.938893903907228378E-16, -1.000000000000000000 ) ) ;
#5340 = ORIENTED_EDGE ( 'NONE', *, *, #10053, .T. ) ;
#5341 = CARTESIAN_POINT ( 'NONE',  ( 3.000000000000000888, 20.65684170206509762, -13.72351598154876484 ) ) ;
#5342 = VECTOR ( 'NONE', #6804, 1000.000000000000000 ) ;
#5343 = DIRECTION ( 'NONE',  ( -1.000000000000000000, 0.000000000000000000, -0.000000000000000000 ) ) ;
#5344 = CARTESIAN_POINT ( 'NONE',  ( -6.589974825828277538, 7.038139701356666222, 10.00000000000000000 ) ) ;
#5345 = EDGE_CURVE ( 'NONE', #9863, #5811, #380, .T. ) ;
#5346 = CARTESIAN_POINT ( 'NONE',  ( 3.000000000000000888, 17.97274125076074114, 13.62355943574025652 ) ) ;
#5347 = FACE_OUTER_BOUND ( 'NONE', #11074, .T. ) ;
#5348 = CIRCLE ( 'NONE', #3581, 9.599999999999997868 ) ;
#5349 = ORIENTED_EDGE ( 'NONE', *, *, #2622, .T. ) ;
#5350 = FACE_OUTER_BOUND ( 'NONE', #396, .T. ) ;
#5351 = ORIENTED_EDGE ( 'NONE', *, *, #8498, .F. ) ;
#5352 = VECTOR ( 'NONE', #3804, 1000.000000000000000 ) ;
#5353 = EDGE_CURVE ( 'NONE', #1896, #5661, #7017, .T. ) ;
#5354 = CARTESIAN_POINT ( 'NONE',  ( -1.790740696106538632, -6.394195405909704810, 3.747395293195558847E-16 ) ) ;
#5355 = DIRECTION ( 'NONE',  ( -1.000000000000000000, -0.000000000000000000, 0.000000000000000000 ) ) ;
#5356 = ORIENTED_EDGE ( 'NONE', *, *, #8247, .T. ) ;
#5357 = AXIS2_PLACEMENT_3D ( 'NONE', #6416, #1039, #911 ) ;
#5358 = CARTESIAN_POINT ( 'NONE',  ( 0.000000000000000000, -2.745295967525840375, -22.83456483164691875 ) ) ;
#5359 = CARTESIAN_POINT ( 'NONE',  ( 0.000000000000000000, 17.71842311621553279, -17.35216073792423330 ) ) ;
#5360 = CARTESIAN_POINT ( 'NONE',  ( 1.022653496104248827, 6.171874473422430007, 10.00000000000000000 ) ) ;
#5361 = CARTESIAN_POINT ( 'NONE',  ( 10.63538685525200478, -4.008487272325076844, 6.857782953271941950E-17 ) ) ;
#5362 = CARTESIAN_POINT ( 'NONE',  ( 0.000000000000000000, -22.47229024614978599, 1.901833551798177036 ) ) ;
#5363 = DIRECTION ( 'NONE',  ( -1.000000000000000000, 0.000000000000000000, -0.000000000000000000 ) ) ;
#5364 = VERTEX_POINT ( 'NONE', #10384 ) ;
#5365 = EDGE_LOOP ( 'NONE', ( #3930, #11022, #6907, #11007 ) ) ;
#5366 = VECTOR ( 'NONE', #4886, 1000.000000000000000 ) ;
#5367 = EDGE_CURVE ( 'NONE', #2865, #4186, #7444, .T. ) ;
#5368 = EDGE_CURVE ( 'NONE', #7212, #5213, #6589, .T. ) ;
#5369 = ORIENTED_EDGE ( 'NONE', *, *, #11033, .F. ) ;
#5370 = CARTESIAN_POINT ( 'NONE',  ( 13.29800827116429929, 3.099979537169774257, 10.00000000000000000 ) ) ;
#5371 = DIRECTION ( 'NONE',  ( 1.000000000000000000, 0.000000000000000000, 0.000000000000000000 ) ) ;
#5372 = CARTESIAN_POINT ( 'NONE',  ( 0.000000000000000000, 0.000000000000000000, 0.000000000000000000 ) ) ;
#5373 = CIRCLE ( 'NONE', #6919, 22.99900000000000588 ) ;
#5374 = CARTESIAN_POINT ( 'NONE',  ( -0.9167995209625431352, 5.268308710424121521, 3.747395293195558847E-16 ) ) ;
#5375 = DIRECTION ( 'NONE',  ( -1.000000000000000000, 0.000000000000000000, -0.000000000000000000 ) ) ;
#5376 = CARTESIAN_POINT ( 'NONE',  ( 3.000000000000000888, 19.74380051311556628, -11.79560690673851475 ) ) ;
#5377 = ORIENTED_EDGE ( 'NONE', *, *, #10475, .T. ) ;
#5378 = ITEM_DEFINED_TRANSFORMATION ( 'NONE', 'NONE', #3728,  #8474 ) ;
#5379 = VERTEX_POINT ( 'NONE', #7377 ) ;
#5380 = DIRECTION ( 'NONE',  ( -1.000000000000000000, 0.000000000000000000, -0.000000000000000000 ) ) ;
#5381 = DIRECTION ( 'NONE',  ( 1.000000000000000000, 0.000000000000000000, 0.000000000000000000 ) ) ;
#5382 = UNCERTAINTY_MEASURE_WITH_UNIT (LENGTH_MEASURE( 1.000000000000000082E-05 ), #10980, 'distance_accuracy_value', 'NONE');
#5383 = DIRECTION ( 'NONE',  ( 1.000000000000000000, 0.000000000000000000, -0.000000000000000000 ) ) ;
#5384 = DIRECTION ( 'NONE',  ( -1.000000000000000000, 0.000000000000000000, 0.000000000000000000 ) ) ;
#5385 = EDGE_CURVE ( 'NONE', #1013, #9776, #12095, .T. ) ;
#5386 = CARTESIAN_POINT ( 'NONE',  ( 16.50000000000000000, 0.000000000000000000, 3.747395293195558847E-16 ) ) ;
#5387 = CARTESIAN_POINT ( 'NONE',  ( -6.451445390047170214, -3.308750875808896819, 6.857782953271941950E-17 ) ) ;
#5388 = DIRECTION ( 'NONE',  ( 0.000000000000000000, 0.000000000000000000, 1.000000000000000000 ) ) ;
#5389 = DIRECTION ( 'NONE',  ( 0.000000000000000000, 0.000000000000000000, 1.000000000000000000 ) ) ;
#5390 = ORIENTED_EDGE ( 'NONE', *, *, #2220, .T. ) ;
#5391 = CARTESIAN_POINT ( 'NONE',  ( 6.563569809674243416, -3.208372544468512721, 10.00000000000000000 ) ) ;
#5392 = ADVANCED_FACE ( 'NONE', ( #7622 ), #100, .T. ) ;
#5393 = VERTEX_POINT ( 'NONE', #11193 ) ;
#5394 = LINE ( 'NONE', #8086, #2071 ) ;
#5395 = VECTOR ( 'NONE', #11635, 1000.000000000000000 ) ;
#5396 = ORIENTED_EDGE ( 'NONE', *, *, #6904, .F. ) ;
#5397 = EDGE_CURVE ( 'NONE', #3932, #4536, #2064, .T. ) ;
#5398 = DIRECTION ( 'NONE',  ( 0.000000000000000000, 0.000000000000000000, -1.000000000000000000 ) ) ;
#5399 = CYLINDRICAL_SURFACE ( 'NONE', #4007, 9.599999999999997868 ) ;
#5400 = CARTESIAN_POINT ( 'NONE',  ( 1.022653496104248827, 6.171874473422430007, 10.00000000000000000 ) ) ;
#5401 = DIRECTION ( 'NONE',  ( 0.000000000000000000, 0.7431448254773909134, 0.6691306063588620123 ) ) ;
#5402 = DIRECTION ( 'NONE',  ( -1.000000000000000000, -0.000000000000000000, -0.000000000000000000 ) ) ;
#5403 = VECTOR ( 'NONE', #10226, 1000.000000000000000 ) ;
#5404 = VERTEX_POINT ( 'NONE', #6470 ) ;
#5405 = CARTESIAN_POINT ( 'NONE',  ( 3.000000000000000888, -14.74749645580022772, 17.06259499759939402 ) ) ;
#5406 = VERTEX_POINT ( 'NONE', #8443 ) ;
#5407 = CARTESIAN_POINT ( 'NONE',  ( 2.084958754360775934, -3.480815169281481047, 3.747395293195558847E-16 ) ) ;
#5408 = DIRECTION ( 'NONE',  ( 0.000000000000000000, 0.000000000000000000, -1.000000000000000000 ) ) ;
#5409 =( LENGTH_UNIT ( ) NAMED_UNIT ( * ) SI_UNIT ( .MILLI., .METRE. ) );
#5410 = ORIENTED_EDGE ( 'NONE', *, *, #4154, .F. ) ;
#5411 = FACE_OUTER_BOUND ( 'NONE', #4924, .T. ) ;
#5412 = AXIS2_PLACEMENT_3D ( 'NONE', #9906, #666, #3364 ) ;
#5413 = CARTESIAN_POINT ( 'NONE',  ( 3.000000000000000888, 24.77821629063821973, -1.039229259764575364 ) ) ;
#5414 = CARTESIAN_POINT ( 'NONE',  ( 3.913389251769919586, -3.458713887698555922, 10.00000000000000000 ) ) ;
#5415 = CARTESIAN_POINT ( 'NONE',  ( 8.143984375791809782, 3.063465613658396425, 6.857782953271941950E-17 ) ) ;
#5416 = CYLINDRICAL_SURFACE ( 'NONE', #4564, 24.80000000000000071 ) ;
#5417 = LINE ( 'NONE', #7178, #7848 ) ;
#5418 = VERTEX_POINT ( 'NONE', #5561 ) ;
#5419 = EDGE_LOOP ( 'NONE', ( #9861, #5874, #327, #960 ) ) ;
#5420 = EDGE_CURVE ( 'NONE', #8541, #7251, #796, .T. ) ;
#5421 = CARTESIAN_POINT ( 'NONE',  ( -8.207979594962568015, -13.19054478262514607, 10.00000000000000000 ) ) ;
#5422 = CARTESIAN_POINT ( 'NONE',  ( 3.000000000000000888, 2.745295967526300451, -22.83456483164686546 ) ) ;
#5423 = DIRECTION ( 'NONE',  ( -1.000000000000000000, 0.000000000000000000, -0.000000000000000000 ) ) ;
#5424 = ADVANCED_FACE ( 'NONE', ( #6533 ), #1884, .T. ) ;
#5425 = CARTESIAN_POINT ( 'NONE',  ( -3.231136241382283725, -5.666136714102345984, 3.747395293195558847E-16 ) ) ;
#5426 = AXIS2_PLACEMENT_3D ( 'NONE', #9820, #10618, #7917 ) ;
#5427 = CARTESIAN_POINT ( 'NONE',  ( 3.000000000000000888, 1.901833551798570721, -22.47229024614975401 ) ) ;
#5428 = CARTESIAN_POINT ( 'NONE',  ( 3.000000000000000888, 0.000000000000000000, 0.000000000000000000 ) ) ;
#5429 = ORIENTED_EDGE ( 'NONE', *, *, #8626, .F. ) ;
#5430 = VERTEX_POINT ( 'NONE', #3790 ) ;
#5431 = CYLINDRICAL_SURFACE ( 'NONE', #6702, 24.80000000000000071 ) ;
#5432 = LINE ( 'NONE', #4584, #10543 ) ;
#5433 = CIRCLE ( 'NONE', #7371, 24.80000000000000071 ) ;
#5434 = DIRECTION ( 'NONE',  ( -1.000000000000000000, 0.000000000000000000, 0.000000000000000000 ) ) ;
#5435 = CYLINDRICAL_SURFACE ( 'NONE', #2019, 5.000000000000000000 ) ;
#5436 = CARTESIAN_POINT ( 'NONE',  ( 1.500000000000000444, -8.645255683529168067, 23.24434456306322616 ) ) ;
#5437 = CARTESIAN_POINT ( 'NONE',  ( 3.000000000000000888, 19.75591328264886215, 10.87771529938168946 ) ) ;
#5438 = CARTESIAN_POINT ( 'NONE',  ( 3.000000000000000888, 20.08719549084865008, 11.20082935824082249 ) ) ;
#5439 = CIRCLE ( 'NONE', #2506, 24.80000000000000071 ) ;
#5440 = ORIENTED_EDGE ( 'NONE', *, *, #4485, .F. ) ;
#5441 = AXIS2_PLACEMENT_3D ( 'NONE', #6285, #7301, #9279 ) ;
#5442 = DIRECTION ( 'NONE',  ( 0.000000000000000000, 0.000000000000000000, 1.000000000000000000 ) ) ;
#5443 = ORIENTED_EDGE ( 'NONE', *, *, #9185, .F. ) ;
#5444 = ORIENTED_EDGE ( 'NONE', *, *, #893, .T. ) ;
#5445 = CARTESIAN_POINT ( 'NONE',  ( 3.120778274233608318, -6.257845451232916467, 10.00000000000000000 ) ) ;
#5446 = ORIENTED_EDGE ( 'NONE', *, *, #7020, .F. ) ;
#5447 = DIRECTION ( 'NONE',  ( 1.000000000000000000, -0.000000000000000000, -0.000000000000000000 ) ) ;
#5448 = ORIENTED_EDGE ( 'NONE', *, *, #3040, .F. ) ;
#5449 = EDGE_CURVE ( 'NONE', #4594, #4467, #9201, .T. ) ;
#5450 = CARTESIAN_POINT ( 'NONE',  ( 0.000000000000000000, -18.80635025205178579, 13.23915371906949012 ) ) ;
#5451 = DIRECTION ( 'NONE',  ( 0.000000000000000000, 0.000000000000000000, 1.000000000000000000 ) ) ;
#5452 = CARTESIAN_POINT ( 'NONE',  ( 10.64229886435067662, -13.41933351754326154, 6.857782953271941950E-17 ) ) ;
#5453 = CYLINDRICAL_SURFACE ( 'NONE', #4146, 9.599999999999994316 ) ;
#5454 = DIRECTION ( 'NONE',  ( 0.000000000000000000, 0.000000000000000000, 1.000000000000000000 ) ) ;
#5455 = ORIENTED_EDGE ( 'NONE', *, *, #1488, .F. ) ;
#5456 = LINE ( 'NONE', #8282, #194 ) ;
#5457 = EDGE_CURVE ( 'NONE', #6518, #7873, #1598, .T. ) ;
#5458 = EDGE_LOOP ( 'NONE', ( #8805, #11887 ) ) ;
#5459 = AXIS2_PLACEMENT_3D ( 'NONE', #1036, #9471, #8316 ) ;
#5460 = VECTOR ( 'NONE', #295, 1000.000000000000000 ) ;
#5461 = EDGE_CURVE ( 'NONE', #6550, #7092, #23, .T. ) ;
#5462 = CARTESIAN_POINT ( 'NONE',  ( -3.663109177303993214, -5.348850660921103284, 3.747395293195558847E-16 ) ) ;
#5463 = AXIS2_PLACEMENT_3D ( 'NONE', #162, #2191, #4771 ) ;
#5464 = CARTESIAN_POINT ( 'NONE',  ( 3.000000000000000888, 4.445336973060856955, 22.56530478845650123 ) ) ;
#5465 = DIRECTION ( 'NONE',  ( 0.000000000000000000, 0.8090169943749485615, -0.5877852522924714718 ) ) ;
#5466 = DIRECTION ( 'NONE',  ( 0.000000000000000000, 0.000000000000000000, 1.000000000000000000 ) ) ;
#5467 = DIRECTION ( 'NONE',  ( 0.000000000000000000, 0.000000000000000000, 1.000000000000000000 ) ) ;
#5468 = DIRECTION ( 'NONE',  ( -1.000000000000000000, 0.000000000000000000, -0.000000000000000000 ) ) ;
#5469 = CARTESIAN_POINT ( 'NONE',  ( 2.919619825260425294, -7.400844473264723611, 6.857782953271941950E-17 ) ) ;
#5470 = LINE ( 'NONE', #2904, #11781 ) ;
#5471 = EDGE_CURVE ( 'NONE', #5393, #11133, #7875, .T. ) ;
#5472 = CARTESIAN_POINT ( 'NONE',  ( 3.000000000000000888, 0.000000000000000000, 0.000000000000000000 ) ) ;
#5473 = EDGE_LOOP ( 'NONE', ( #3276, #10899, #10857, #10611 ) ) ;
#5474 = EDGE_LOOP ( 'NONE', ( #9773, #6429, #5755, #9988 ) ) ;
#5475 = ORIENTED_EDGE ( 'NONE', *, *, #7048, .F. ) ;
#5476 = CIRCLE ( 'NONE', #4508, 22.99899999999999523 ) ;
#5477 = CARTESIAN_POINT ( 'NONE',  ( 0.000000000000000000, -1.556492618230473468, -24.75110766671653906 ) ) ;
#5478 = CARTESIAN_POINT ( 'NONE',  ( -6.430932688512554840, -6.885836206078318256, 10.00000000000000000 ) ) ;
#5479 = AXIS2_PLACEMENT_3D ( 'NONE', #8032, #7104, #10855 ) ;
#5480 = CARTESIAN_POINT ( 'NONE',  ( 0.000000000000000000, 19.10918332567978695, -15.80756504416672215 ) ) ;
#5481 = EDGE_CURVE ( 'NONE', #1256, #1804, #3748, .T. ) ;
#5482 = CYLINDRICAL_SURFACE ( 'NONE', #10128, 9.599999999999997868 ) ;
#5483 = STYLED_ITEM ( 'NONE', ( #6622 ), #1326 ) ;
#5484 = CARTESIAN_POINT ( 'NONE',  ( 7.078846155421574693, 8.354583459611243157, 3.747395293195558847E-16 ) ) ;
#5485 = CARTESIAN_POINT ( 'NONE',  ( 1.500000000000000444, -24.75110766671653195, 1.556492618230556513 ) ) ;
#5486 = EDGE_CURVE ( 'NONE', #2776, #10367, #10587, .T. ) ;
#5487 = CARTESIAN_POINT ( 'NONE',  ( 0.000000000000000000, 0.000000000000000000, 0.000000000000000000 ) ) ;
#5488 = ORIENTED_EDGE ( 'NONE', *, *, #11879, .T. ) ;
#5489 = VECTOR ( 'NONE', #11455, 1000.000000000000000 ) ;
#5490 = DIRECTION ( 'NONE',  ( -1.000000000000000000, 0.000000000000000000, 0.000000000000000000 ) ) ;
#5491 = EDGE_LOOP ( 'NONE', ( #5906, #9390, #10562, #5013 ) ) ;
#5492 = ORIENTED_EDGE ( 'NONE', *, *, #5198, .T. ) ;
#5493 = CARTESIAN_POINT ( 'NONE',  ( -1.103316172498963521, -16.73802372459124044, 6.857782953271941950E-17 ) ) ;
#5494 = ORIENTED_EDGE ( 'NONE', *, *, #7004, .T. ) ;
#5495 = CYLINDRICAL_SURFACE ( 'NONE', #10815, 3.500000000000000000 ) ;
#5496 = CYLINDRICAL_SURFACE ( 'NONE', #7809, 9.599999999999997868 ) ;
#5497 = EDGE_CURVE ( 'NONE', #4594, #7105, #8040, .T. ) ;
#5498 = AXIS2_PLACEMENT_3D ( 'NONE', #10074, #2490, #5186 ) ;
#5499 =( NAMED_UNIT ( * ) SI_UNIT ( $, .STERADIAN. ) SOLID_ANGLE_UNIT ( ) );
#5500 = UNCERTAINTY_MEASURE_WITH_UNIT (LENGTH_MEASURE( 1.000000000000000082E-05 ), #2591, 'distance_accuracy_value', 'NONE');
#5501 = FACE_OUTER_BOUND ( 'NONE', #11842, .T. ) ;
#5502 = COLOUR_RGB ( '', 0.31764706, 0.68627451, 0.89019608) ;
#5503 = DIRECTION ( 'NONE',  ( -1.000000000000000000, 0.000000000000000000, 0.000000000000000000 ) ) ;
#5504 = CARTESIAN_POINT ( 'NONE',  ( -15.05755265055531034, -0.4891349978715467950, 3.747395293195558847E-16 ) ) ;
#5505 = CARTESIAN_POINT ( 'NONE',  ( -7.040021908109678428, -0.4595208068204874041, 6.857782953271941950E-17 ) ) ;
#5506 = VECTOR ( 'NONE', #1909, 1000.000000000000000 ) ;
#5507 = CARTESIAN_POINT ( 'NONE',  ( 0.000000000000000000, 0.000000000000000000, 0.000000000000000000 ) ) ;
#5508 = ORIENTED_EDGE ( 'NONE', *, *, #2420, .F. ) ;
#5509 = VERTEX_POINT ( 'NONE', #5861 ) ;
#5510 = CARTESIAN_POINT ( 'NONE',  ( 3.000000000000000888, -21.96011696265487600, -5.135568396240250522 ) ) ;
#5511 = AXIS2_PLACEMENT_3D ( 'NONE', #2890, #1056, #7589 ) ;
#5512 = ORIENTED_EDGE ( 'NONE', *, *, #9512, .T. ) ;
#5513 = ORIENTED_EDGE ( 'NONE', *, *, #1143, .T. ) ;
#5514 = CARTESIAN_POINT ( 'NONE',  ( -2.296015608618633852, -6.188270089872266233, 10.00000000000000000 ) ) ;
#5515 = DIRECTION ( 'NONE',  ( -1.000000000000000000, 0.000000000000000000, -0.000000000000000000 ) ) ;
#5516 = VERTEX_POINT ( 'NONE', #10746 ) ;
#5517 = CIRCLE ( 'NONE', #9615, 9.599999999999997868 ) ;
#5518 = AXIS2_PLACEMENT_3D ( 'NONE', #12057, #7466, #10229 ) ;
#5519 = CARTESIAN_POINT ( 'NONE',  ( 0.000000000000000000, 0.000000000000000000, -5.000000000000000000 ) ) ;
#5520 = DIRECTION ( 'NONE',  ( -1.000000000000000000, -0.000000000000000000, -0.000000000000000000 ) ) ;
#5521 = CARTESIAN_POINT ( 'NONE',  ( 3.666996827460253350, 4.772409917195344242, 10.00000000000000000 ) ) ;
#5522 = FACE_OUTER_BOUND ( 'NONE', #8514, .T. ) ;
#5523 = DIRECTION ( 'NONE',  ( -1.000000000000000000, -0.000000000000000000, -0.000000000000000000 ) ) ;
#5524 = ORIENTED_EDGE ( 'NONE', *, *, #1143, .F. ) ;
#5525 = ORIENTED_EDGE ( 'NONE', *, *, #6921, .F. ) ;
#5526 = CIRCLE ( 'NONE', #8603, 9.599999999999997868 ) ;
#5527 = DIRECTION ( 'NONE',  ( 0.000000000000000000, 0.9945218953682729568, 0.1045284632676570929 ) ) ;
#5528 = ORIENTED_EDGE ( 'NONE', *, *, #4525, .T. ) ;
#5529 =( GEOMETRIC_REPRESENTATION_CONTEXT ( 3 ) GLOBAL_UNCERTAINTY_ASSIGNED_CONTEXT ( ( #5382 ) ) GLOBAL_UNIT_ASSIGNED_CONTEXT ( ( #10980, #10861, #1490 ) ) REPRESENTATION_CONTEXT ( 'NONE', 'WORKASPACE' ) );
#5530 = CARTESIAN_POINT ( 'NONE',  ( -5.962113107391269651, -1.426310550302858582, 3.747395293195558847E-16 ) ) ;
#5531 = DIRECTION ( 'NONE',  ( 0.000000000000000000, 0.000000000000000000, 1.000000000000000000 ) ) ;
#5532 = VERTEX_POINT ( 'NONE', #3963 ) ;
#5533 = DIRECTION ( 'NONE',  ( -1.000000000000000000, 0.000000000000000000, 0.000000000000000000 ) ) ;
#5534 = EDGE_CURVE ( 'NONE', #5028, #11239, #6864, .T. ) ;
#5535 = DIRECTION ( 'NONE',  ( -1.000000000000000000, -0.000000000000000000, 0.000000000000000000 ) ) ;
#5536 = DIRECTION ( 'NONE',  ( 0.000000000000000000, 0.000000000000000000, 1.000000000000000000 ) ) ;
#5537 = CARTESIAN_POINT ( 'NONE',  ( -5.924299593718516554, 3.297400215539475710, 6.857782953271941950E-17 ) ) ;
#5538 = DIRECTION ( 'NONE',  ( -1.000000000000000000, -0.000000000000000000, 0.000000000000000000 ) ) ;
#5539 = ADVANCED_FACE ( 'NONE', ( #4145 ), #7811, .T. ) ;
#5540 = DIRECTION ( 'NONE',  ( 0.000000000000000000, 0.000000000000000000, 1.000000000000000000 ) ) ;
#5541 = CIRCLE ( 'NONE', #9060, 9.599999999999997868 ) ;
#5542 = AXIS2_PLACEMENT_3D ( 'NONE', #3736, #7461, #237 ) ;
#5543 = EDGE_LOOP ( 'NONE', ( #8955, #4283, #8016, #8171 ) ) ;
#5544 = ORIENTED_EDGE ( 'NONE', *, *, #767, .F. ) ;
#5545 = ORIENTED_EDGE ( 'NONE', *, *, #10467, .F. ) ;
#5546 = CIRCLE ( 'NONE', #4182, 24.80000000000000071 ) ;
#5547 = CYLINDRICAL_SURFACE ( 'NONE', #11711, 9.599999999999997868 ) ;
#5548 = CARTESIAN_POINT ( 'NONE',  ( 0.6578947103914143391, -9.792230064638474119, 10.00000000000000000 ) ) ;
#5549 = EDGE_CURVE ( 'NONE', #2329, #9635, #3351, .T. ) ;
#5550 = DIRECTION ( 'NONE',  ( 0.000000000000000000, 0.000000000000000000, 1.000000000000000000 ) ) ;
#5551 = CARTESIAN_POINT ( 'NONE',  ( 3.000000000000000888, 24.45282072769606430, -4.135161237383341515 ) ) ;
#5552 = EDGE_CURVE ( 'NONE', #1145, #5516, #1385, .T. ) ;
#5553 = CARTESIAN_POINT ( 'NONE',  ( 8.913847851857145344, -5.129921849437907078, 3.747395293195558847E-16 ) ) ;
#5554 = FACE_OUTER_BOUND ( 'NONE', #6606, .T. ) ;
#5555 = VECTOR ( 'NONE', #11890, 1000.000000000000000 ) ;
#5556 = FACE_OUTER_BOUND ( 'NONE', #546, .T. ) ;
#5557 = ORIENTED_EDGE ( 'NONE', *, *, #2509, .T. ) ;
#5558 = EDGE_LOOP ( 'NONE', ( #11910, #8655, #7756, #5283 ) ) ;
#5559 = ORIENTED_EDGE ( 'NONE', *, *, #11105, .T. ) ;
#5560 = CARTESIAN_POINT ( 'NONE',  ( 1.499999999999999556, -6.668524164681463695, -23.88662356770121775 ) ) ;
#5561 = CARTESIAN_POINT ( 'NONE',  ( -11.50000000000000178, 0.000000000000000000, 4.000000000000000000 ) ) ;
#5562 = CIRCLE ( 'NONE', #2041, 9.599999999999997868 ) ;
#5563 = CYLINDRICAL_SURFACE ( 'NONE', #565, 22.99899999999999878 ) ;
#5564 = CARTESIAN_POINT ( 'NONE',  ( 3.000000000000000888, 6.532525787311267429, -21.58580335785669746 ) ) ;
#5565 = DIRECTION ( 'NONE',  ( 0.000000000000000000, -0.7431448254773861395, -0.6691306063588672304 ) ) ;
#5566 = CARTESIAN_POINT ( 'NONE',  ( 10.01890055165174864, -12.63311126014528796, 3.747395293195558847E-16 ) ) ;
#5567 = CARTESIAN_POINT ( 'NONE',  ( -5.248573321596925467, 4.168074790661427720, 6.857782953271941950E-17 ) ) ;
#5568 = CARTESIAN_POINT ( 'NONE',  ( 3.000000000000000888, 0.000000000000000000, 0.000000000000000000 ) ) ;
#5569 = CIRCLE ( 'NONE', #2438, 22.99900000000000588 ) ;
#5570 = EDGE_LOOP ( 'NONE', ( #646, #11574, #8830, #3452 ) ) ;
#5571 = VERTEX_POINT ( 'NONE', #4021 ) ;
#5572 = CYLINDRICAL_SURFACE ( 'NONE', #1193, 22.99899999999999878 ) ;
#5573 = ORIENTED_EDGE ( 'NONE', *, *, #4060, .F. ) ;
#5574 = VERTEX_POINT ( 'NONE', #5119 ) ;
#5575 = CARTESIAN_POINT ( 'NONE',  ( 0.5697670706242778937, -3.781298318517896551, 10.00000000000000000 ) ) ;
#5576 = ADVANCED_FACE ( 'NONE', ( #3224 ), #5001, .T. ) ;
#5577 = CARTESIAN_POINT ( 'NONE',  ( 3.000000000000000888, 0.000000000000000000, 0.000000000000000000 ) ) ;
#5578 = EDGE_LOOP ( 'NONE', ( #5429, #7755, #8269, #7982 ) ) ;
#5579 = CARTESIAN_POINT ( 'NONE',  ( 3.000000000000000888, -4.135161237383746524, 24.45282072769599679 ) ) ;
#5580 = CARTESIAN_POINT ( 'NONE',  ( 0.000000000000000000, -11.67026512804534022, -19.29833442572371638 ) ) ;
#5581 = CARTESIAN_POINT ( 'NONE',  ( 2.529667540517110513, -4.392173529266737653, 10.00000000000000000 ) ) ;
#5582 =( NAMED_UNIT ( * ) PLANE_ANGLE_UNIT ( ) SI_UNIT ( $, .RADIAN. ) );
#5583 = EDGE_CURVE ( 'NONE', #11368, #308, #8859, .T. ) ;
#5584 = CARTESIAN_POINT ( 'NONE',  ( -19.99999999999999645, 0.000000000000000000, 20.00000000000000000 ) ) ;
#5585 = ORIENTED_EDGE ( 'NONE', *, *, #1301, .F. ) ;
#5586 = ORIENTED_EDGE ( 'NONE', *, *, #4189, .T. ) ;
#5587 = CARTESIAN_POINT ( 'NONE',  ( -10.00000000000000000, 0.000000000000000000, 0.000000000000000000 ) ) ;
#5588 = EDGE_LOOP ( 'NONE', ( #5989, #753, #4804, #11557 ) ) ;
#5589 = CIRCLE ( 'NONE', #9488, 9.599999999999997868 ) ;
#5590 = CARTESIAN_POINT ( 'NONE',  ( -5.541928854458315179, -2.884958602215172085, 3.747395293195558847E-16 ) ) ;
#5591 = PLANE ( 'NONE',  #2264 ) ;
#5592 = DIRECTION ( 'NONE',  ( -1.000000000000000000, -0.000000000000000000, -0.000000000000000000 ) ) ;
#5593 = FACE_OUTER_BOUND ( 'NONE', #1901, .T. ) ;
#5594 = CARTESIAN_POINT ( 'NONE',  ( -16.06046882360140060, -0.5196555361422392494, 10.00000000000000000 ) ) ;
#5595 = VECTOR ( 'NONE', #3441, 1000.000000000000000 ) ;
#5596 = CARTESIAN_POINT ( 'NONE',  ( 3.534825977509324257, -7.171832907601985774, 6.857782953271941950E-17 ) ) ;
#5597 = CYLINDRICAL_SURFACE ( 'NONE', #644, 9.599999999999997868 ) ;
#5598 = CARTESIAN_POINT ( 'NONE',  ( 0.000000000000000000, 0.000000000000000000, 0.000000000000000000 ) ) ;
#5599 = ORIENTED_EDGE ( 'NONE', *, *, #11296, .T. ) ;
#5600 = VERTEX_POINT ( 'NONE', #8681 ) ;
#5601 = VERTEX_POINT ( 'NONE', #7749 ) ;
#5602 = AXIS2_PLACEMENT_3D ( 'NONE', #7213, #6318, #9247 ) ;
#5603 = DIRECTION ( 'NONE',  ( -1.000000000000000000, -0.000000000000000000, -0.000000000000000000 ) ) ;
#5604 = CARTESIAN_POINT ( 'NONE',  ( -7.402161455537875412, -5.702533393948235663, 10.00000000000000000 ) ) ;
#5605 = FACE_OUTER_BOUND ( 'NONE', #7094, .T. ) ;
#5606 = CARTESIAN_POINT ( 'NONE',  ( 1.499999999999999556, 1.556492618230641556, 24.75110766671652485 ) ) ;
#5607 = CARTESIAN_POINT ( 'NONE',  ( -7.402161455537873636, -5.702533393948970186, 3.747395293195558847E-16 ) ) ;
#5608 = EDGE_CURVE ( 'NONE', #7701, #3870, #1507, .T. ) ;
#5609 = DIRECTION ( 'NONE',  ( 1.000000000000000000, 0.000000000000000000, 0.000000000000000000 ) ) ;
#5610 = DIRECTION ( 'NONE',  ( -1.000000000000000000, 0.000000000000000000, 0.000000000000000000 ) ) ;
#5611 = ORIENTED_EDGE ( 'NONE', *, *, #3530, .T. ) ;
#5612 = PRODUCT_DEFINITION ( 'UNKNOWN', '', #6461, #8318 ) ;
#5613 = ORIENTED_EDGE ( 'NONE', *, *, #4038, .T. ) ;
#5614 = EDGE_CURVE ( 'NONE', #3056, #1694, #2368, .T. ) ;
#5615 = ORIENTED_EDGE ( 'NONE', *, *, #6579, .F. ) ;
#5616 = DIRECTION ( 'NONE',  ( 1.000000000000000000, 0.000000000000000000, -0.000000000000000000 ) ) ;
#5617 = EDGE_CURVE ( 'NONE', #9078, #117, #2495, .T. ) ;
#5618 = DIRECTION ( 'NONE',  ( -1.000000000000000000, 0.000000000000000000, 0.000000000000000000 ) ) ;
#5619 = CARTESIAN_POINT ( 'NONE',  ( 1.499999999999999556, 3.623565124517435176, -24.53384959170453783 ) ) ;
#5620 = PLANE ( 'NONE',  #750 ) ;
#5621 = CIRCLE ( 'NONE', #1908, 22.99899999999999878 ) ;
#5622 = DIRECTION ( 'NONE',  ( 0.000000000000000000, -0.5877852522924797984, 0.8090169943749426773 ) ) ;
#5623 = CARTESIAN_POINT ( 'NONE',  ( -14.60057116351879714, -4.165219547604622541, 3.747395293195558847E-16 ) ) ;
#5624 = CARTESIAN_POINT ( 'NONE',  ( -6.211147023100837217, 2.816369743025007644, 6.857782953271941950E-17 ) ) ;
#5625 = DIRECTION ( 'NONE',  ( 0.000000000000000000, 0.000000000000000000, 1.000000000000000000 ) ) ;
#5626 = ORIENTED_EDGE ( 'NONE', *, *, #3161, .T. ) ;
#5627 = ORIENTED_EDGE ( 'NONE', *, *, #10391, .T. ) ;
#5628 = CARTESIAN_POINT ( 'NONE',  ( 0.000000000000000000, 0.000000000000000000, 4.000000000000000000 ) ) ;
#5629 = ORIENTED_EDGE ( 'NONE', *, *, #8383, .F. ) ;
#5630 = AXIS2_PLACEMENT_3D ( 'NONE', #1067, #1916, #8 ) ;
#5631 = ORIENTED_EDGE ( 'NONE', *, *, #3414, .T. ) ;
#5632 = CARTESIAN_POINT ( 'NONE',  ( 3.000000000000000888, 0.000000000000000000, 0.000000000000000000 ) ) ;
#5633 = DIRECTION ( 'NONE',  ( -1.000000000000000000, -0.000000000000000000, 0.000000000000000000 ) ) ;
#5634 = ORIENTED_EDGE ( 'NONE', *, *, #4478, .F. ) ;
#5635 = DIRECTION ( 'NONE',  ( 0.000000000000000000, 0.000000000000000000, 1.000000000000000000 ) ) ;
#5636 = ADVANCED_FACE ( 'NONE', ( #11911 ), #5431, .T. ) ;
#5637 = CARTESIAN_POINT ( 'NONE',  ( 0.000000000000000000, -21.58580335785672233, -6.532525787311189269 ) ) ;
#5638 = CARTESIAN_POINT ( 'NONE',  ( 2.004495162477544223, 5.838205294495796949, 10.00000000000000000 ) ) ;
#5639 = AXIS2_PLACEMENT_3D ( 'NONE', #103, #8319, #7448 ) ;
#5640 = AXIS2_PLACEMENT_3D ( 'NONE', #144, #10495, #4755 ) ;
#5641 = CARTESIAN_POINT ( 'NONE',  ( 0.000000000000000000, 6.779701584703026640, -21.97702544527751201 ) ) ;
#5642 = EDGE_CURVE ( 'NONE', #6844, #1972, #6124, .T. ) ;
#5643 = CARTESIAN_POINT ( 'NONE',  ( 3.000000000000000888, -13.23915371906968019, 18.80635025205165078 ) ) ;
#5644 = EDGE_LOOP ( 'NONE', ( #1111, #2786, #3536, #5756 ) ) ;
#5645 = CYLINDRICAL_SURFACE ( 'NONE', #8223, 9.599999999999999645 ) ;
#5646 = VERTEX_POINT ( 'NONE', #4395 ) ;
#5647 = CARTESIAN_POINT ( 'NONE',  ( 1.629745903656676820, 14.14889381255350287, 10.00000000000000000 ) ) ;
#5648 = CIRCLE ( 'NONE', #4861, 24.80000000000000071 ) ;
#5649 = AXIS2_PLACEMENT_3D ( 'NONE', #3329, #4992, #1372 ) ;
#5650 = FACE_OUTER_BOUND ( 'NONE', #9973, .T. ) ;
#5651 =( NAMED_UNIT ( * ) SI_UNIT ( $, .STERADIAN. ) SOLID_ANGLE_UNIT ( ) );
#5652 = ADVANCED_FACE ( 'NONE', ( #8129 ), #9160, .T. ) ;
#5653 = CARTESIAN_POINT ( 'NONE',  ( 0.000000000000000000, 0.000000000000000000, 0.000000000000000000 ) ) ;
#5654 = DIRECTION ( 'NONE',  ( 0.000000000000000000, 0.000000000000000000, -1.000000000000000000 ) ) ;
#5655 = CARTESIAN_POINT ( 'NONE',  ( -10.11701526667144257, 11.92482893257633947, 10.00000000000000000 ) ) ;
#5656 = CARTESIAN_POINT ( 'NONE',  ( -2.570438583093345386, 5.934334910739564428, 6.857782953271941950E-17 ) ) ;
#5657 = CARTESIAN_POINT ( 'NONE',  ( 3.000000000000000888, 12.88318129270179035, 18.51065745848382349 ) ) ;
#5658 = AXIS2_PLACEMENT_3D ( 'NONE', #2497, #719, #8190 ) ;
#5659 = VECTOR ( 'NONE', #5270, 1000.000000000000000 ) ;
#5660 = CARTESIAN_POINT ( 'NONE',  ( 17.49999999999999645, 0.000000000000000000, 6.857782953271941950E-17 ) ) ;
#5661 = VERTEX_POINT ( 'NONE', #778 ) ;
#5662 = EDGE_LOOP ( 'NONE', ( #9174, #4316, #6497, #6410 ) ) ;
#5663 = CYLINDRICAL_SURFACE ( 'NONE', #726, 9.599999999999997868 ) ;
#5664 = CARTESIAN_POINT ( 'NONE',  ( 8.282588618526579793, 7.043362411858248073, 10.00000000000000000 ) ) ;
#5665 = CIRCLE ( 'NONE', #10745, 22.99899999999999523 ) ;
#5666 = FACE_OUTER_BOUND ( 'NONE', #3912, .T. ) ;
#5667 = CIRCLE ( 'NONE', #175, 22.99900000000000233 ) ;
#5668 = CARTESIAN_POINT ( 'NONE',  ( 6.391761267590965190, 8.940137919805573929, 3.747395293195558847E-16 ) ) ;
#5669 = CARTESIAN_POINT ( 'NONE',  ( 4.516389116325773223, 1.247036727255508515, 3.747395293195558847E-16 ) ) ;
#5670 = DIRECTION ( 'NONE',  ( 0.000000000000000000, 0.000000000000000000, 1.000000000000000000 ) ) ;
#5671 = VERTEX_POINT ( 'NONE', #7255 ) ;
#5672 = AXIS2_PLACEMENT_3D ( 'NONE', #3101, #4875, #457 ) ;
#5673 = ORIENTED_EDGE ( 'NONE', *, *, #2522, .F. ) ;
#5674 = VERTEX_POINT ( 'NONE', #4517 ) ;
#5675 = CIRCLE ( 'NONE', #4496, 9.599999999999997868 ) ;
#5676 = ORIENTED_EDGE ( 'NONE', *, *, #4870, .F. ) ;
#5677 = CARTESIAN_POINT ( 'NONE',  ( 1.499999999999999556, -24.77821629063822328, 1.039229259764403501 ) ) ;
#5678 = CARTESIAN_POINT ( 'NONE',  ( 3.000000000000000888, -22.54798042742717357, 9.142421143074578538 ) ) ;
#5679 = DIRECTION ( 'NONE',  ( 0.000000000000000000, 0.000000000000000000, 1.000000000000000000 ) ) ;
#5680 = FACE_OUTER_BOUND ( 'NONE', #632, .T. ) ;
#5681 = AXIS2_PLACEMENT_3D ( 'NONE', #4624, #2905, #12075 ) ;
#5682 = CARTESIAN_POINT ( 'NONE',  ( 0.000000000000000000, 15.80756504416717334, -19.10918332567941036 ) ) ;
#5683 = AXIS2_PLACEMENT_3D ( 'NONE', #8261, #8197, #3613 ) ;
#5684 = EDGE_CURVE ( 'NONE', #4987, #4256, #8187, .T. ) ;
#5685 = AXIS2_PLACEMENT_3D ( 'NONE', #9186, #7535, #811 ) ;
#5686 = CARTESIAN_POINT ( 'NONE',  ( 7.795318149608630343, -14.02504990431079612, 3.747395293195558847E-16 ) ) ;
#5687 = CARTESIAN_POINT ( 'NONE',  ( -10.00000000000000000, 0.000000000000000000, 0.000000000000000000 ) ) ;
#5688 = AXIS2_PLACEMENT_3D ( 'NONE', #4029, #8568, #166 ) ;
#5689 = EDGE_CURVE ( 'NONE', #845, #7676, #5142, .T. ) ;
#5690 = DIRECTION ( 'NONE',  ( -1.000000000000000000, 0.000000000000000000, -0.000000000000000000 ) ) ;
#5691 = CARTESIAN_POINT ( 'NONE',  ( -22.00000000000000000, 0.000000000000000000, 3.000000000000000000 ) ) ;
#5692 = ORIENTED_EDGE ( 'NONE', *, *, #8230, .F. ) ;
#5693 = ORIENTED_EDGE ( 'NONE', *, *, #466, .F. ) ;
#5694 = CARTESIAN_POINT ( 'NONE',  ( 0.000000000000000000, -21.76479567747236743, -7.432877647175426539 ) ) ;
#5695 = AXIS2_PLACEMENT_3D ( 'NONE', #6736, #11329, #5825 ) ;
#5696 = ORIENTED_EDGE ( 'NONE', *, *, #11744, .F. ) ;
#5697 = CIRCLE ( 'NONE', #4719, 22.99899999999999878 ) ;
#5698 = DIRECTION ( 'NONE',  ( -1.000000000000000000, -0.000000000000000000, 0.000000000000000000 ) ) ;
#5699 = CIRCLE ( 'NONE', #2756, 9.599999999999999645 ) ;
#5700 = CARTESIAN_POINT ( 'NONE',  ( 3.000000000000000888, -19.74380051311548456, 11.79560690673865331 ) ) ;
#5701 = ORIENTED_EDGE ( 'NONE', *, *, #4040, .F. ) ;
#5702 = EDGE_CURVE ( 'NONE', #8206, #11050, #7683, .T. ) ;
#5703 = DIRECTION ( 'NONE',  ( 1.000000000000000000, 0.000000000000000000, 0.000000000000000000 ) ) ;
#5704 = CARTESIAN_POINT ( 'NONE',  ( 0.000000000000000000, -2.062268319295719632, 22.90635393027945454 ) ) ;
#5705 = CARTESIAN_POINT ( 'NONE',  ( -10.11701526667143725, 11.92482893257633414, 6.857782953271941950E-17 ) ) ;
#5706 = CIRCLE ( 'NONE', #17, 22.99899999999999878 ) ;
#5707 = PRODUCT_DEFINITION_SHAPE ( 'NONE', 'NONE',  #12118 ) ;
#5708 = CARTESIAN_POINT ( 'NONE',  ( 3.000000000000000000, 0.000000000000000000, 10.00000000000000000 ) ) ;
#5709 = AXIS2_PLACEMENT_3D ( 'NONE', #8352, #1731, #1981 ) ;
#5710 = CARTESIAN_POINT ( 'NONE',  ( 3.000000000000000888, -9.667200211209964422, 20.86861857134731579 ) ) ;
#5711 = ORIENTED_EDGE ( 'NONE', *, *, #6149, .T. ) ;
#5712 = DIRECTION ( 'NONE',  ( -1.000000000000000000, -0.000000000000000000, 0.000000000000000000 ) ) ;
#5713 = ORIENTED_EDGE ( 'NONE', *, *, #9658, .T. ) ;
#5714 = EDGE_CURVE ( 'NONE', #9333, #730, #6515, .T. ) ;
#5715 = CARTESIAN_POINT ( 'NONE',  ( 11.04976219204224996, -11.79656285005915350, 10.00000000000000000 ) ) ;
#5716 = AXIS2_PLACEMENT_3D ( 'NONE', #874, #1906, #2703 ) ;
#5717 = VECTOR ( 'NONE', #8758, 1000.000000000000000 ) ;
#5718 = CARTESIAN_POINT ( 'NONE',  ( 1.499999999999999556, 3.623565124517106995, 24.53384959170458757 ) ) ;
#5719 = ORIENTED_EDGE ( 'NONE', *, *, #6137, .F. ) ;
#5720 = CIRCLE ( 'NONE', #9976, 9.599999999999999645 ) ;
#5721 = EDGE_CURVE ( 'NONE', #4653, #9467, #8066, .T. ) ;
#5722 = CARTESIAN_POINT ( 'NONE',  ( 0.000000000000000000, 0.000000000000000000, 0.000000000000000000 ) ) ;
#5723 = FACE_OUTER_BOUND ( 'NONE', #2267, .T. ) ;
#5724 = CARTESIAN_POINT ( 'NONE',  ( 3.017784444055084947, -16.62017357425736463, 10.00000000000000000 ) ) ;
#5725 = CARTESIAN_POINT ( 'NONE',  ( 3.000000000000000888, -22.99643626497956461, -0.3433949777334098785 ) ) ;
#5726 = DIRECTION ( 'NONE',  ( 0.000000000000000000, 0.5000000000000011102, -0.8660254037844381525 ) ) ;
#5727 = DIRECTION ( 'NONE',  ( 0.000000000000000000, -0.8090169943749526693, 0.5877852522924661427 ) ) ;
#5728 = MECHANICAL_DESIGN_GEOMETRIC_PRESENTATION_REPRESENTATION (  '', ( #8851 ), #431 ) ;
#5729 = EDGE_LOOP ( 'NONE', ( #1817, #11958, #5440, #8358 ) ) ;
#5730 = CARTESIAN_POINT ( 'NONE',  ( -10.00000000000000000, 0.000000000000000000, 0.000000000000000000 ) ) ;
#5731 = ORIENTED_EDGE ( 'NONE', *, *, #10793, .F. ) ;
#5732 = CARTESIAN_POINT ( 'NONE',  ( 3.000000000000000888, -12.88318129270191825, 18.51065745848373822 ) ) ;
#5733 = CARTESIAN_POINT ( 'NONE',  ( -3.141381368647836236, 10.98006565327106543, 10.00000000000000000 ) ) ;
#5734 = EDGE_CURVE ( 'NONE', #2005, #1648, #10622, .T. ) ;
#5735 = AXIS2_PLACEMENT_3D ( 'NONE', #8465, #3807, #482 ) ;
#5736 = FACE_BOUND ( 'NONE', #11005, .T. ) ;
#5737 = CARTESIAN_POINT ( 'NONE',  ( -8.109405675832187299, 8.372220220304370741, 3.747395293195558847E-16 ) ) ;
#5738 = CIRCLE ( 'NONE', #7490, 9.599999999999997868 ) ;
#5739 =( GEOMETRIC_REPRESENTATION_CONTEXT ( 3 ) GLOBAL_UNCERTAINTY_ASSIGNED_CONTEXT ( ( #7317 ) ) GLOBAL_UNIT_ASSIGNED_CONTEXT ( ( #9205, #7487, #8355 ) ) REPRESENTATION_CONTEXT ( 'NONE', 'WORKASPACE' ) );
#5740 = CARTESIAN_POINT ( 'NONE',  ( -1.124919223378054722, -13.71093750358708085, 6.857782953271941950E-17 ) ) ;
#5741 = DIRECTION ( 'NONE',  ( 0.000000000000000000, 0.000000000000000000, 1.000000000000000000 ) ) ;
#5742 = ORIENTED_EDGE ( 'NONE', *, *, #7867, .T. ) ;
#5743 = EDGE_CURVE ( 'NONE', #10686, #6311, #8273, .T. ) ;
#5744 = CIRCLE ( 'NONE', #9647, 9.599999999999996092 ) ;
#5745 = ORIENTED_EDGE ( 'NONE', *, *, #9824, .T. ) ;
#5746 = VERTEX_POINT ( 'NONE', #8442 ) ;
#5747 = CARTESIAN_POINT ( 'NONE',  ( 0.000000000000000000, -8.645255683528846546, -23.24434456306333985 ) ) ;
#5748 = CARTESIAN_POINT ( 'NONE',  ( 3.000000000000000888, 21.96011696265491153, -5.135568396240103084 ) ) ;
#5749 = EDGE_LOOP ( 'NONE', ( #9483, #9538, #1046, #11051 ) ) ;
#5750 = FACE_OUTER_BOUND ( 'NONE', #4750, .T. ) ;
#5751 = DIRECTION ( 'NONE',  ( -1.000000000000000000, -1.445602896647339163E-16, 0.000000000000000000 ) ) ;
#5752 = CARTESIAN_POINT ( 'NONE',  ( 0.000000000000000000, 0.000000000000000000, 0.000000000000000000 ) ) ;
#5753 = CARTESIAN_POINT ( 'NONE',  ( -6.423942855642367000, 13.01866063961475461, 3.747395293195558847E-16 ) ) ;
#5754 = CARTESIAN_POINT ( 'NONE',  ( 0.000000000000000000, 0.000000000000000000, 0.000000000000000000 ) ) ;
#5755 = ORIENTED_EDGE ( 'NONE', *, *, #11999, .T. ) ;
#5756 = ORIENTED_EDGE ( 'NONE', *, *, #851, .T. ) ;
#5757 = CARTESIAN_POINT ( 'NONE',  ( -13.43906451854578954, -9.301052350413227643, 10.00000000000000000 ) ) ;
#5758 = ORIENTED_EDGE ( 'NONE', *, *, #11915, .F. ) ;
#5759 = CARTESIAN_POINT ( 'NONE',  ( 2.084958754360777711, -3.480815169282206689, 10.00000000000000000 ) ) ;
#5760 = FACE_OUTER_BOUND ( 'NONE', #10530, .T. ) ;
#5761 = EDGE_LOOP ( 'NONE', ( #10491, #2107, #11106, #9941 ) ) ;
#5762 = ADVANCED_FACE ( 'NONE', ( #2866 ), #5495, .T. ) ;
#5763 = FACE_OUTER_BOUND ( 'NONE', #10094, .T. ) ;
#5764 = CARTESIAN_POINT ( 'NONE',  ( 0.000000000000000000, 0.3433949777331667397, 22.99643626497956816 ) ) ;
#5765 = CARTESIAN_POINT ( 'NONE',  ( 1.124919223378051392, -13.78906249641291559, 6.857782953271941950E-17 ) ) ;
#5766 = AXIS2_PLACEMENT_3D ( 'NONE', #4000, #7726, #2841 ) ;
#5767 = EDGE_CURVE ( 'NONE', #11802, #9240, #6532, .T. ) ;
#5768 = CARTESIAN_POINT ( 'NONE',  ( 3.000000000000000888, 7.402892494506579268, -21.30300407174355115 ) ) ;
#5769 = FACE_OUTER_BOUND ( 'NONE', #11568, .T. ) ;
#5770 = ORIENTED_EDGE ( 'NONE', *, *, #11476, .T. ) ;
#5771 = EDGE_LOOP ( 'NONE', ( #7967, #8725, #4899, #11416 ) ) ;
#5772 = LINE ( 'NONE', #4788, #5489 ) ;
#5773 = VERTEX_POINT ( 'NONE', #10137 ) ;
#5774 = EDGE_CURVE ( 'NONE', #3600, #11784, #5541, .T. ) ;
#5775 = CARTESIAN_POINT ( 'NONE',  ( 13.53515989517831919, -0.2218654272303337005, 10.00000000000000000 ) ) ;
#5776 = ADVANCED_FACE ( 'NONE', ( #848 ), #4583, .T. ) ;
#5777 = DIRECTION ( 'NONE',  ( -1.000000000000000000, -0.000000000000000000, 0.000000000000000000 ) ) ;
#5778 = EDGE_CURVE ( 'NONE', #1706, #5601, #9835, .T. ) ;
#5779 = CARTESIAN_POINT ( 'NONE',  ( 14.52660474336492236, -9.366294961249355566, 6.857782953271941950E-17 ) ) ;
#5780 = FACE_OUTER_BOUND ( 'NONE', #10870, .T. ) ;
#5781 = CARTESIAN_POINT ( 'NONE',  ( 3.000000000000000888, -9.589108953448036488, 20.41249101028208202 ) ) ;
#5782 = CARTESIAN_POINT ( 'NONE',  ( -5.414455899168761022, -12.47541146649038879, 10.00000000000000000 ) ) ;
#5783 = CARTESIAN_POINT ( 'NONE',  ( 0.000000000000000000, -4.240409074144249502, 22.15038895030647836 ) ) ;
#5784 = CARTESIAN_POINT ( 'NONE',  ( -14.61026919807147095, 3.159152207411756397, 3.747395293195558847E-16 ) ) ;
#5785 = CARTESIAN_POINT ( 'NONE',  ( 3.000000000000000888, 2.811977935937781670, 22.37663021667345120 ) ) ;
#5786 = ORIENTED_EDGE ( 'NONE', *, *, #7277, .T. ) ;
#5787 = CIRCLE ( 'NONE', #5190, 9.599999999999999645 ) ;
#5788 = DIRECTION ( 'NONE',  ( -1.000000000000000000, -0.000000000000000000, 0.000000000000000000 ) ) ;
#5789 = VERTEX_POINT ( 'NONE', #2807 ) ;
#5790 = DIRECTION ( 'NONE',  ( 0.000000000000000000, 0.9510565162951543083, -0.3090169943749450643 ) ) ;
#5791 = CARTESIAN_POINT ( 'NONE',  ( 7.536008357046525497, 0.2705779428718255719, 10.00000000000000000 ) ) ;
#5792 = CARTESIAN_POINT ( 'NONE',  ( 0.000000000000000000, 0.000000000000000000, 0.000000000000000000 ) ) ;
#5793 = VECTOR ( 'NONE', #2695, 1000.000000000000000 ) ;
#5794 = CARTESIAN_POINT ( 'NONE',  ( -3.909826107003197215, 8.641065831729468627, 10.00000000000000000 ) ) ;
#5795 = CARTESIAN_POINT ( 'NONE',  ( 11.20109743375191691, 9.815261043521076090, 6.857782953271941950E-17 ) ) ;
#5796 = DIRECTION ( 'NONE',  ( -1.000000000000000000, 0.000000000000000000, 0.000000000000000000 ) ) ;
#5797 = ORIENTED_EDGE ( 'NONE', *, *, #8678, .F. ) ;
#5798 = EDGE_CURVE ( 'NONE', #7882, #7859, #10266, .T. ) ;
#5799 = AXIS2_PLACEMENT_3D ( 'NONE', #2826, #10282, #11268 ) ;
#5800 = ORIENTED_EDGE ( 'NONE', *, *, #8268, .F. ) ;
#5801 = CARTESIAN_POINT ( 'NONE',  ( 3.000000000000000888, 0.000000000000000000, 0.000000000000000000 ) ) ;
#5802 = DIRECTION ( 'NONE',  ( -1.000000000000000000, -0.000000000000000000, 0.000000000000000000 ) ) ;
#5803 = EDGE_LOOP ( 'NONE', ( #9732, #8793, #2145, #8999 ) ) ;
#5804 = CARTESIAN_POINT ( 'NONE',  ( 0.000000000000000000, 0.000000000000000000, 0.000000000000000000 ) ) ;
#5805 = DIRECTION ( 'NONE',  ( 0.07332096784668425127, 0.9973083954695386444, 3.060346140701604533E-16 ) ) ;
#5806 = ADVANCED_FACE ( 'NONE', ( #7565 ), #2676, .T. ) ;
#5807 = DIRECTION ( 'NONE',  ( 0.000000000000000000, 0.000000000000000000, 1.000000000000000000 ) ) ;
#5808 = CARTESIAN_POINT ( 'NONE',  ( -1.035167565893234443, -12.71157708251009133, 3.747395293195558847E-16 ) ) ;
#5809 = CYLINDRICAL_SURFACE ( 'NONE', #4099, 22.99899999999999878 ) ;
#5810 = ORIENTED_EDGE ( 'NONE', *, *, #1903, .F. ) ;
#5811 = VERTEX_POINT ( 'NONE', #152 ) ;
#5812 = SHAPE_REPRESENTATION_RELATIONSHIP ( 'NONE' , 'NONE' ,  #7555, #7312 ) ;
#5813 = CARTESIAN_POINT ( 'NONE',  ( -11.80455809908110432, -11.41585333555581983, 10.00000000000000000 ) ) ;
#5814 = ORIENTED_EDGE ( 'NONE', *, *, #9278, .T. ) ;
#5815 = DIRECTION ( 'NONE',  ( 0.000000000000000000, -0.3090169943749349613, -0.9510565162951576390 ) ) ;
#5816 = CARTESIAN_POINT ( 'NONE',  ( 3.000000000000000888, 16.85990652506920995, -15.64281154287580655 ) ) ;
#5817 = LINE ( 'NONE', #3675, #5403 ) ;
#5818 = VERTEX_POINT ( 'NONE', #12093 ) ;
#5819 = CARTESIAN_POINT ( 'NONE',  ( 3.000000000000000000, 0.000000000000000000, 18.49999999999999645 ) ) ;
#5820 = DIRECTION ( 'NONE',  ( 0.000000000000000000, 0.000000000000000000, 1.000000000000000000 ) ) ;
#5821 = CARTESIAN_POINT ( 'NONE',  ( -14.19814495527598730, 7.008511237308412412, 6.857782953271941950E-17 ) ) ;
#5822 = AXIS2_PLACEMENT_3D ( 'NONE', #10550, #8424, #6756 ) ;
#5823 = FACE_OUTER_BOUND ( 'NONE', #8440, .T. ) ;
#5824 = ORIENTED_EDGE ( 'NONE', *, *, #4258, .T. ) ;
#5825 = DIRECTION ( 'NONE',  ( 0.000000000000000000, 0.000000000000000000, 1.000000000000000000 ) ) ;
#5826 = VECTOR ( 'NONE', #8532, 1000.000000000000000 ) ;
#5827 = ORIENTED_EDGE ( 'NONE', *, *, #3972, .T. ) ;
#5828 = VERTEX_POINT ( 'NONE', #11250 ) ;
#5829 = CARTESIAN_POINT ( 'NONE',  ( 3.000000000000000888, -22.90635393027944744, -2.062268319295799568 ) ) ;
#5830 = ORIENTED_EDGE ( 'NONE', *, *, #7268, .T. ) ;
#5831 = CARTESIAN_POINT ( 'NONE',  ( 13.03626601087043113, 4.193914020169875911, 10.00000000000000000 ) ) ;
#5832 = EDGE_CURVE ( 'NONE', #622, #8206, #2740, .T. ) ;
#5833 = DIRECTION ( 'NONE',  ( -1.000000000000000000, 0.000000000000000000, -0.000000000000000000 ) ) ;
#5834 = CARTESIAN_POINT ( 'NONE',  ( 17.46093749967478104, -1.431715403549062460, 6.857782953271941950E-17 ) ) ;
#5835 = AXIS2_PLACEMENT_3D ( 'NONE', #7878, #3172, #3052 ) ;
#5836 = DIRECTION ( 'NONE',  ( 0.000000000000000000, 0.000000000000000000, 1.000000000000000000 ) ) ;
#5837 = DIRECTION ( 'NONE',  ( -1.000000000000000000, -0.000000000000000000, -0.000000000000000000 ) ) ;
#5838 = CARTESIAN_POINT ( 'NONE',  ( -3.406233159845097891, 11.94786423299365197, 10.00000000000000000 ) ) ;
#5839 = CARTESIAN_POINT ( 'NONE',  ( 0.000000000000000000, 0.000000000000000000, 0.000000000000000000 ) ) ;
#5840 = CARTESIAN_POINT ( 'NONE',  ( -11.99326810842395474, 8.590522060507202795, 3.747395293195558847E-16 ) ) ;
#5841 = EDGE_CURVE ( 'NONE', #4846, #7440, #5738, .T. ) ;
#5842 = DIRECTION ( 'NONE',  ( -1.000000000000000000, -0.000000000000000000, -0.000000000000000000 ) ) ;
#5843 = EDGE_CURVE ( 'NONE', #10367, #1329, #1821, .T. ) ;
#5844 = CARTESIAN_POINT ( 'NONE',  ( 1.499999999999999556, 11.02759168516775290, -22.21333432029552668 ) ) ;
#5845 = AXIS2_PLACEMENT_3D ( 'NONE', #2669, #895, #8302 ) ;
#5846 = PRESENTATION_LAYER_ASSIGNMENT (  '', '', ( #9152 ) ) ;
#5847 = ORIENTED_EDGE ( 'NONE', *, *, #6292, .T. ) ;
#5848 = VERTEX_POINT ( 'NONE', #5747 ) ;
#5849 = CARTESIAN_POINT ( 'NONE',  ( 3.000000000000000888, -21.30300407174367905, 7.402892494506218668 ) ) ;
#5850 = CARTESIAN_POINT ( 'NONE',  ( 4.623190192904714557, -5.402202315098911356, 10.00000000000000000 ) ) ;
#5851 = LINE ( 'NONE', #6700, #362 ) ;
#5852 = CARTESIAN_POINT ( 'NONE',  ( -4.368568794346924022, -9.638580752213403713, 10.00000000000000000 ) ) ;
#5853 = EDGE_CURVE ( 'NONE', #5055, #11545, #8502, .T. ) ;
#5854 = CARTESIAN_POINT ( 'NONE',  ( -13.43906451854462603, -9.301052350413224090, 6.857782953271941950E-17 ) ) ;
#5855 = CYLINDRICAL_SURFACE ( 'NONE', #9769, 9.599999999999997868 ) ;
#5856 = VERTEX_POINT ( 'NONE', #906 ) ;
#5857 = ORIENTED_EDGE ( 'NONE', *, *, #7856, .T. ) ;
#5858 = AXIS2_PLACEMENT_3D ( 'NONE', #10943, #1519, #10021 ) ;
#5859 = CARTESIAN_POINT ( 'NONE',  ( 0.000000000000000000, 23.24434456306337538, -8.645255683528764834 ) ) ;
#5860 = EDGE_CURVE ( 'NONE', #4143, #5993, #4563, .T. ) ;
#5861 = CARTESIAN_POINT ( 'NONE',  ( 3.000000000000000888, -21.14796121233203152, 9.039786367038763260 ) ) ;
#5862 = DIRECTION ( 'NONE',  ( -1.000000000000000000, -0.000000000000000000, -0.000000000000000000 ) ) ;
#5863 = CARTESIAN_POINT ( 'NONE',  ( -10.00000000000000000, 0.000000000000000000, 0.000000000000000000 ) ) ;
#5864 = ADVANCED_FACE ( 'NONE', ( #4820 ), #963, .T. ) ;
#5865 = CARTESIAN_POINT ( 'NONE',  ( 7.316052646047088714, -7.060001943526879487, 3.747395293195558847E-16 ) ) ;
#5866 = EDGE_CURVE ( 'NONE', #5789, #8927, #4749, .T. ) ;
#5867 = CIRCLE ( 'NONE', #7021, 24.80000000000000071 ) ;
#5868 = DIRECTION ( 'NONE',  ( 0.000000000000000000, 0.5877852522924690293, 0.8090169943749504489 ) ) ;
#5869 = ORIENTED_EDGE ( 'NONE', *, *, #6882, .T. ) ;
#5870 = ORIENTED_EDGE ( 'NONE', *, *, #213, .F. ) ;
#5871 = PRODUCT_CONTEXT ( 'NONE', #7781, 'mechanical' ) ;
#5872 = CARTESIAN_POINT ( 'NONE',  ( 0.07364157424580704270, -3.751631698233870438, 3.747395293195558847E-16 ) ) ;
#5873 = EDGE_CURVE ( 'NONE', #5271, #3286, #6853, .T. ) ;
#5874 = ORIENTED_EDGE ( 'NONE', *, *, #10061, .F. ) ;
#5875 = CARTESIAN_POINT ( 'NONE',  ( 3.000000000000000888, 6.668524164681629784, 23.88662356770117867 ) ) ;
#5876 = CARTESIAN_POINT ( 'NONE',  ( -1.500000000000000222, 1.836970198721030181E-16, 0.000000000000000000 ) ) ;
#5877 = FACE_OUTER_BOUND ( 'NONE', #5761, .T. ) ;
#5878 = ORIENTED_EDGE ( 'NONE', *, *, #8983, .F. ) ;
#5879 = VECTOR ( 'NONE', #9559, 1000.000000000000000 ) ;
#5880 = DIRECTION ( 'NONE',  ( 0.000000000000000000, -0.8090169943749525583, 0.5877852522924661427 ) ) ;
#5881 = AXIS2_PLACEMENT_3D ( 'NONE', #8806, #3001, #2130 ) ;
#5882 = DIRECTION ( 'NONE',  ( -1.000000000000000000, 0.000000000000000000, -0.000000000000000000 ) ) ;
#5883 = CARTESIAN_POINT ( 'NONE',  ( -5.683926142426733108, 14.39978054689283660, 6.857782953271941950E-17 ) ) ;
#5884 = ORIENTED_EDGE ( 'NONE', *, *, #10915, .F. ) ;
#5885 = CYLINDRICAL_SURFACE ( 'NONE', #6278, 9.599999999999997868 ) ;
#5886 = AXIS2_PLACEMENT_3D ( 'NONE', #10201, #7437, #959 ) ;
#5887 = ORIENTED_EDGE ( 'NONE', *, *, #2480, .F. ) ;
#5888 = CARTESIAN_POINT ( 'NONE',  ( 3.000000000000000888, -18.80635025205160815, -13.23915371906974592 ) ) ;
#5889 = AXIS2_PLACEMENT_3D ( 'NONE', #11749, #6246, #3437 ) ;
#5890 = ORIENTED_EDGE ( 'NONE', *, *, #1621, .T. ) ;
#5891 = CARTESIAN_POINT ( 'NONE',  ( 2.103398428914359908, -12.69820342197951035, 10.00000000000000000 ) ) ;
#5892 = DIRECTION ( 'NONE',  ( -1.000000000000000000, 0.000000000000000000, -0.000000000000000000 ) ) ;
#5894 = VECTOR ( 'NONE', #5375, 1000.000000000000000 ) ;
#5893 = DIRECTION ( 'NONE',  ( 0.000000000000000000, 1.000000000000000000, 3.491481338843133355E-15 ) ) ;
#5895 = AXIS2_PLACEMENT_3D ( 'NONE', #5437, #9167, #785 ) ;
#5896 = CARTESIAN_POINT ( 'NONE',  ( 0.000000000000000000, 4.240409074144393387, -22.15038895030644639 ) ) ;
#5897 = CARTESIAN_POINT ( 'NONE',  ( 5.334478431285540445, 14.15651896542077104, 10.00000000000000000 ) ) ;
#5898 = AXIS2_PLACEMENT_3D ( 'NONE', #6034, #8618, #463 ) ;
#5899 = CARTESIAN_POINT ( 'NONE',  ( 3.000000000000000888, -11.02759168516730881, -22.21333432029575050 ) ) ;
#5900 = CARTESIAN_POINT ( 'NONE',  ( 10.01890055165174864, -12.63311126014528796, 3.747395293195558847E-16 ) ) ;
#5901 = FACE_OUTER_BOUND ( 'NONE', #8272, .T. ) ;
#5902 = DIRECTION ( 'NONE',  ( -1.000000000000000000, 0.000000000000000000, -0.000000000000000000 ) ) ;
#5903 = MECHANICAL_DESIGN_GEOMETRIC_PRESENTATION_REPRESENTATION (  '', ( #6101 ), #8652 ) ;
#5904 = PRODUCT_DEFINITION_SHAPE ( 'NONE', 'NONE',  #12121 ) ;
#5905 = CIRCLE ( 'NONE', #3760, 20.00000000000000000 ) ;
#5906 = ORIENTED_EDGE ( 'NONE', *, *, #8689, .F. ) ;
#5907 = DIRECTION ( 'NONE',  ( 0.000000000000000000, 0.6691306063588543518, 0.7431448254773976858 ) ) ;
#5908 = CARTESIAN_POINT ( 'NONE',  ( 3.656769781543558917, 7.172433557890307121, 10.00000000000000000 ) ) ;
#5909 = DIRECTION ( 'NONE',  ( 1.000000000000000000, 0.000000000000000000, 0.000000000000000000 ) ) ;
#5910 = ADVANCED_FACE ( 'NONE', ( #4080 ), #566, .T. ) ;
#5911 = ADVANCED_FACE ( 'NONE', ( #4879 ), #8738, .T. ) ;
#5912 = CARTESIAN_POINT ( 'NONE',  ( 0.000000000000000000, 0.000000000000000000, -5.000000000000000000 ) ) ;
#5913 = AXIS2_PLACEMENT_3D ( 'NONE', #4840, #8643, #2086 ) ;
#5914 = CARTESIAN_POINT ( 'NONE',  ( -8.665663522307777811, -5.581295667939715877, 10.00000000000000000 ) ) ;
#5915 = AXIS2_PLACEMENT_3D ( 'NONE', #7260, #2444, #7081 ) ;
#5916 = CARTESIAN_POINT ( 'NONE',  ( -11.61414229320030067, -6.453515506896104981, 6.857782953271941950E-17 ) ) ;
#5917 = SURFACE_STYLE_FILL_AREA ( #9758 ) ;
#5918 = CARTESIAN_POINT ( 'NONE',  ( 22.00000000000000000, 2.694222958124176809E-15, 20.00000000000000000 ) ) ;
#5919 = ORIENTED_EDGE ( 'NONE', *, *, #4438, .T. ) ;
#5920 = VERTEX_POINT ( 'NONE', #8795 ) ;
#5921 = EDGE_CURVE ( 'NONE', #2834, #4353, #4159, .T. ) ;
#5922 = CARTESIAN_POINT ( 'NONE',  ( 0.000000000000000000, 21.96011696265484403, 5.135568396240393518 ) ) ;
#5923 = DIRECTION ( 'NONE',  ( -1.000000000000000000, 0.000000000000000000, 0.000000000000000000 ) ) ;
#5924 = EDGE_CURVE ( 'NONE', #10265, #2252, #10502, .T. ) ;
#5925 = CARTESIAN_POINT ( 'NONE',  ( 3.000000000000000888, 9.589108953447894379, 20.41249101028215307 ) ) ;
#5926 = AXIS2_PLACEMENT_3D ( 'NONE', #10183, #11232, #11102 ) ;
#5927 = DIRECTION ( 'NONE',  ( -0.000000000000000000, -0.000000000000000000, 1.000000000000000000 ) ) ;
#5928 = CARTESIAN_POINT ( 'NONE',  ( 3.053028024665286111, -9.450988318041344982, 3.747395293195558847E-16 ) ) ;
#5929 = AXIS2_PLACEMENT_3D ( 'NONE', #6055, #5998, #357 ) ;
#5930 = DIRECTION ( 'NONE',  ( 1.000000000000000000, 1.445602896647338917E-16, 0.000000000000000000 ) ) ;
#5931 = ORIENTED_EDGE ( 'NONE', *, *, #10093, .F. ) ;
#5932 = VECTOR ( 'NONE', #6411, 1000.000000000000000 ) ;
#5933 = VERTEX_POINT ( 'NONE', #11546 ) ;
#5934 = AXIS2_PLACEMENT_3D ( 'NONE', #5632, #6548, #11386 ) ;
#5935 = APPLICATION_PROTOCOL_DEFINITION ( 'draft international standard', 'automotive_design', 1998, #9663 ) ;
#5936 = CARTESIAN_POINT ( 'NONE',  ( 4.165359127293308816, 14.58480927028733554, 10.00000000000000000 ) ) ;
#5937 = VERTEX_POINT ( 'NONE', #2118 ) ;
#5938 = CARTESIAN_POINT ( 'NONE',  ( 7.014224211608840243, -15.49593329755746218, 6.857782953271941950E-17 ) ) ;
#5939 = FACE_OUTER_BOUND ( 'NONE', #7029, .T. ) ;
#5940 = CARTESIAN_POINT ( 'NONE',  ( 3.000000000000000888, -13.79477846460808799, 18.40266524480583854 ) ) ;
#5941 = CIRCLE ( 'NONE', #5357, 24.80000000000000071 ) ;
#5942 = LINE ( 'NONE', #9668, #8922 ) ;
#5943 = ORIENTED_EDGE ( 'NONE', *, *, #10443, .T. ) ;
#5944 = PLANE ( 'NONE',  #4360 ) ;
#5945 = CARTESIAN_POINT ( 'NONE',  ( 0.000000000000000000, 13.62355943574019435, 17.97274125076078732 ) ) ;
#5946 = CARTESIAN_POINT ( 'NONE',  ( 12.50121531544688480, -6.953993600215016002, 6.857782953271941950E-17 ) ) ;
#5947 = ORIENTED_EDGE ( 'NONE', *, *, #3605, .T. ) ;
#5948 = CARTESIAN_POINT ( 'NONE',  ( 3.000000000000000888, -22.21333432029571142, 11.02759168516737276 ) ) ;
#5949 = DIRECTION ( 'NONE',  ( -1.000000000000000000, -0.000000000000000000, -0.000000000000000000 ) ) ;
#5950 = ORIENTED_EDGE ( 'NONE', *, *, #6577, .F. ) ;
#5951 = EDGE_CURVE ( 'NONE', #474, #7150, #5330, .T. ) ;
#5952 = CARTESIAN_POINT ( 'NONE',  ( 10.51453309316909568, -0.3307463982597985686, 10.00000000000000000 ) ) ;
#5953 = CARTESIAN_POINT ( 'NONE',  ( 3.000000000000000888, -11.67026512804560134, 19.29833442572355651 ) ) ;
#5954 = ORIENTED_EDGE ( 'NONE', *, *, #1050, .F. ) ;
#5955 = VECTOR ( 'NONE', #8480, 1000.000000000000000 ) ;
#5956 = DIRECTION ( 'NONE',  ( -1.000000000000000000, 0.000000000000000000, 0.000000000000000000 ) ) ;
#5957 = EDGE_CURVE ( 'NONE', #8820, #2346, #1618, .T. ) ;
#5958 = DIRECTION ( 'NONE',  ( -1.000000000000000000, 0.000000000000000000, -0.000000000000000000 ) ) ;
#5959 = CARTESIAN_POINT ( 'NONE',  ( 12.50121531544689013, -6.953993600215019555, 10.00000000000000000 ) ) ;
#5960 =( LENGTH_UNIT ( ) NAMED_UNIT ( * ) SI_UNIT ( .MILLI., .METRE. ) );
#5961 = CARTESIAN_POINT ( 'NONE',  ( 15.00667705184753764, -6.512453894250635145, 3.747395293195558847E-16 ) ) ;
#5962 = DIRECTION ( 'NONE',  ( -1.000000000000000000, -0.000000000000000000, -0.000000000000000000 ) ) ;
#5963 = DIRECTION ( 'NONE',  ( 1.000000000000000000, 0.000000000000000000, 0.000000000000000000 ) ) ;
#5964 = ORIENTED_EDGE ( 'NONE', *, *, #6830, .F. ) ;
#5965 = VERTEX_POINT ( 'NONE', #5859 ) ;
#5966 = ORIENTED_EDGE ( 'NONE', *, *, #10256, .F. ) ;
#5967 = CARTESIAN_POINT ( 'NONE',  ( -19.99999999999999645, 0.000000000000000000, 20.00000000000000000 ) ) ;
#5968 = CARTESIAN_POINT ( 'NONE',  ( 0.000000000000000000, -10.87771529938148518, -19.75591328264897228 ) ) ;
#5969 = FACE_OUTER_BOUND ( 'NONE', #3359, .T. ) ;
#5970 = CARTESIAN_POINT ( 'NONE',  ( -9.960937504979712642, 0.8181230654450121209, 10.00000000000000000 ) ) ;
#5971 = AXIS2_PLACEMENT_3D ( 'NONE', #2408, #506, #1433 ) ;
#5972 = CARTESIAN_POINT ( 'NONE',  ( 4.479449988082533807, -13.21383449271837840, 6.857782953271941950E-17 ) ) ;
#5973 = CARTESIAN_POINT ( 'NONE',  ( 0.000000000000000000, 2.062268319295869734, -22.90635393027944389 ) ) ;
#5974 = CARTESIAN_POINT ( 'NONE',  ( 1.500000000000000444, 8.645255683529011748, 23.24434456306327945 ) ) ;
#5975 = ORIENTED_EDGE ( 'NONE', *, *, #11334, .T. ) ;
#5976 = VERTEX_POINT ( 'NONE', #11769 ) ;
#5977 = ORIENTED_EDGE ( 'NONE', *, *, #4678, .T. ) ;
#5978 = CARTESIAN_POINT ( 'NONE',  ( 3.000000000000000888, -22.47229024614978599, 1.901833551798177036 ) ) ;
#5979 = CIRCLE ( 'NONE', #3240, 9.599999999999996092 ) ;
#5980 = DIRECTION ( 'NONE',  ( -1.000000000000000000, 0.000000000000000000, -0.000000000000000000 ) ) ;
#5981 = EDGE_CURVE ( 'NONE', #9480, #8232, #7748, .T. ) ;
#5982 = LINE ( 'NONE', #9766, #2313 ) ;
#5983 = DIRECTION ( 'NONE',  ( -1.000000000000000000, 0.000000000000000000, 0.000000000000000000 ) ) ;
#5984 = CARTESIAN_POINT ( 'NONE',  ( -5.773631947676829412, 9.989728373610901713, 3.747395293195558847E-16 ) ) ;
#5985 = ADVANCED_FACE ( 'NONE', ( #5056 ), #10563, .T. ) ;
#5986 = CIRCLE ( 'NONE', #5799, 22.99899999999999878 ) ;
#5987 = EDGE_CURVE ( 'NONE', #4735, #11471, #7065, .T. ) ;
#5988 = CARTESIAN_POINT ( 'NONE',  ( 1.500000000000000222, 0.000000000000000000, -15.00000000000000000 ) ) ;
#5989 = ORIENTED_EDGE ( 'NONE', *, *, #4255, .T. ) ;
#5990 = ORIENTED_EDGE ( 'NONE', *, *, #462, .T. ) ;
#5991 = EDGE_CURVE ( 'NONE', #11333, #5773, #634, .T. ) ;
#5992 = CARTESIAN_POINT ( 'NONE',  ( 13.99323099383125069, 4.495563823643928814, 10.00000000000000000 ) ) ;
#5993 = VERTEX_POINT ( 'NONE', #6888 ) ;
#5994 = DIRECTION ( 'NONE',  ( -1.000000000000000000, 0.000000000000000000, 0.000000000000000000 ) ) ;
#5995 = DIRECTION ( 'NONE',  ( 0.000000000000000000, -0.9945218953682721796, -0.1045284632676635739 ) ) ;
#5996 = CYLINDRICAL_SURFACE ( 'NONE', #9505, 22.99899999999999878 ) ;
#5997 = ORIENTED_EDGE ( 'NONE', *, *, #5174, .T. ) ;
#5998 = DIRECTION ( 'NONE',  ( -1.000000000000000000, -0.000000000000000000, -0.000000000000000000 ) ) ;
#5999 = LINE ( 'NONE', #8704, #5717 ) ;
#6000 = CARTESIAN_POINT ( 'NONE',  ( 11.50231346626665285, 1.508968394323198847, 6.857782953271941950E-17 ) ) ;
#6001 = PRODUCT ( 'BR-102', 'BR-102', '', ( #8747 ) ) ;
#6002 = ORIENTED_EDGE ( 'NONE', *, *, #5987, .T. ) ;
#6003 = DIRECTION ( 'NONE',  ( 1.000000000000000000, 0.000000000000000000, -0.000000000000000000 ) ) ;
#6004 = DIRECTION ( 'NONE',  ( -1.000000000000000000, 0.000000000000000000, -0.000000000000000000 ) ) ;
#6005 = ORIENTED_EDGE ( 'NONE', *, *, #1168, .F. ) ;
#6006 = CARTESIAN_POINT ( 'NONE',  ( -6.430932688512554840, -6.885836206078318256, 10.00000000000000000 ) ) ;
#6007 = EDGE_CURVE ( 'NONE', #9404, #6354, #3265, .T. ) ;
#6008 = CARTESIAN_POINT ( 'NONE',  ( 3.000000000000000888, 0.000000000000000000, 0.000000000000000000 ) ) ;
#6009 =( NAMED_UNIT ( * ) PLANE_ANGLE_UNIT ( ) SI_UNIT ( $, .RADIAN. ) );
#6010 = DIRECTION ( 'NONE',  ( -1.000000000000000000, 0.000000000000000000, 0.000000000000000000 ) ) ;
#6011 = DIRECTION ( 'NONE',  ( 0.000000000000000000, 0.5877852522924690293, 0.8090169943749505599 ) ) ;
#6012 = CARTESIAN_POINT ( 'NONE',  ( -12.06849956494803600, -5.462025159505909500, 10.00000000000000000 ) ) ;
#6013 = EDGE_CURVE ( 'NONE', #1910, #2001, #7361, .T. ) ;
#6014 = CIRCLE ( 'NONE', #11507, 9.599999999999996092 ) ;
#6015 = DIRECTION ( 'NONE',  ( 0.000000000000000000, 0.2079116908177597312, -0.9781476007338056888 ) ) ;
#6016 = CARTESIAN_POINT ( 'NONE',  ( 16.50000000000000000, 0.000000000000000000, 3.747395293195558847E-16 ) ) ;
#6017 = CYLINDRICAL_SURFACE ( 'NONE', #8811, 24.80000000000000071 ) ;
#6018 = ORIENTED_EDGE ( 'NONE', *, *, #5608, .T. ) ;
#6019 = CARTESIAN_POINT ( 'NONE',  ( 0.000000000000000000, 6.532525787310969001, 21.58580335785678983 ) ) ;
#6020 = ORIENTED_EDGE ( 'NONE', *, *, #9243, .F. ) ;
#6021 = ORIENTED_EDGE ( 'NONE', *, *, #170, .T. ) ;
#6022 = ADVANCED_FACE ( 'NONE', ( #9928 ), #8617, .T. ) ;
#6023 = VECTOR ( 'NONE', #8479, 1000.000000000000000 ) ;
#6024 = DIRECTION ( 'NONE',  ( 0.000000000000000000, 0.000000000000000000, 1.000000000000000000 ) ) ;
#6025 = CARTESIAN_POINT ( 'NONE',  ( 0.000000000000000000, 22.37663021667344054, -2.811977935937859385 ) ) ;
#6026 = DIRECTION ( 'NONE',  ( 0.000000000000000000, -0.9945218953682744001, 0.1045284632676437564 ) ) ;
#6027 = CARTESIAN_POINT ( 'NONE',  ( -8.209791827104817585, -6.297951179201753291, 10.00000000000000000 ) ) ;
#6028 = CARTESIAN_POINT ( 'NONE',  ( 8.025946968469181542, -7.769110617520081696, 6.857782953271941950E-17 ) ) ;
#6029 = CARTESIAN_POINT ( 'NONE',  ( 3.000000000000000888, 20.08719549084880640, -11.20082935824054182 ) ) ;
#6030 = ORIENTED_EDGE ( 'NONE', *, *, #2461, .F. ) ;
#6031 = VECTOR ( 'NONE', #11180, 1000.000000000000000 ) ;
#6032 = ORIENTED_EDGE ( 'NONE', *, *, #2795, .F. ) ;
#6033 = ORIENTED_EDGE ( 'NONE', *, *, #9609, .F. ) ;
#6034 = CARTESIAN_POINT ( 'NONE',  ( 0.000000000000000000, -22.37663021667341923, -2.811977935938010376 ) ) ;
#6035 = CIRCLE ( 'NONE', #360, 9.599999999999997868 ) ;
#6036 =( NAMED_UNIT ( * ) PLANE_ANGLE_UNIT ( ) SI_UNIT ( $, .RADIAN. ) );
#6037 = CARTESIAN_POINT ( 'NONE',  ( 1.499999999999999556, -4.135161237383400135, -24.45282072769605364 ) ) ;
#6038 = DIRECTION ( 'NONE',  ( 0.000000000000000000, 0.000000000000000000, 1.000000000000000000 ) ) ;
#6039 = CARTESIAN_POINT ( 'NONE',  ( -1.307086582042907619, 11.26718560147321213, 3.747395293195558847E-16 ) ) ;
#6040 = CARTESIAN_POINT ( 'NONE',  ( 3.000000000000000888, 0.000000000000000000, 0.000000000000000000 ) ) ;
#6041 = AXIS2_PLACEMENT_3D ( 'NONE', #7195, #9905, #11064 ) ;
#6042 = CYLINDRICAL_SURFACE ( 'NONE', #6444, 24.80000000000000071 ) ;
#6043 = AXIS2_PLACEMENT_3D ( 'NONE', #966, #5862, #2006 ) ;
#6044 = ORIENTED_EDGE ( 'NONE', *, *, #2312, .F. ) ;
#6045 = ORIENTED_EDGE ( 'NONE', *, *, #7918, .F. ) ;
#6046 = ITEM_DEFINED_TRANSFORMATION ( 'NONE', 'NONE', #1185,  #8474 ) ;
#6047 = CARTESIAN_POINT ( 'NONE',  ( -0.3972327064967878796, 12.29993208790120640, 10.00000000000000000 ) ) ;
#6048 = AXIS2_PLACEMENT_3D ( 'NONE', #9420, #8452, #2934 ) ;
#6049 = ORIENTED_EDGE ( 'NONE', *, *, #5534, .F. ) ;
#6050 = CARTESIAN_POINT ( 'NONE',  ( 3.000000000000000888, 15.42759117534407309, -16.45023496161649845 ) ) ;
#6051 = DIRECTION ( 'NONE',  ( 0.000000000000000000, 0.000000000000000000, 1.000000000000000000 ) ) ;
#6052 = CARTESIAN_POINT ( 'NONE',  ( 3.000000000000000888, 11.02759168516775112, -22.21333432029552668 ) ) ;
#6053 = ORIENTED_EDGE ( 'NONE', *, *, #8983, .T. ) ;
#6054 = ADVANCED_FACE ( 'NONE', ( #3962 ), #5284, .T. ) ;
#6055 = CARTESIAN_POINT ( 'NONE',  ( 3.000000000000000888, 0.000000000000000000, 0.000000000000000000 ) ) ;
#6056 = ADVANCED_FACE ( 'NONE', ( #3048 ), #2986, .T. ) ;
#6057 = CIRCLE ( 'NONE', #776, 24.80000000000000071 ) ;
#6058 = CYLINDRICAL_SURFACE ( 'NONE', #7062, 22.99899999999999878 ) ;
#6059 = CARTESIAN_POINT ( 'NONE',  ( 5.893263639826756162, 6.717612500731040548, 6.857782953271941950E-17 ) ) ;
#6060 = EDGE_LOOP ( 'NONE', ( #9184, #2638, #3471, #2492 ) ) ;
#6061 = CARTESIAN_POINT ( 'NONE',  ( 0.000000000000000000, -9.589108953448036488, 20.41249101028208202 ) ) ;
#6062 = ORIENTED_EDGE ( 'NONE', *, *, #11744, .T. ) ;
#6063 = CARTESIAN_POINT ( 'NONE',  ( 3.000000000000000888, 0.000000000000000000, 0.000000000000000000 ) ) ;
#6064 = AXIS2_PLACEMENT_3D ( 'NONE', #11049, #1985, #7359 ) ;
#6065 = ORIENTED_EDGE ( 'NONE', *, *, #9457, .F. ) ;
#6066 = CARTESIAN_POINT ( 'NONE',  ( -11.15100792855599110, -5.055838994807845488, 10.00000000000000000 ) ) ;
#6067 = ADVANCED_FACE ( 'NONE', ( #2182, #8546 ), #1190, .T. ) ;
#6068 = ORIENTED_EDGE ( 'NONE', *, *, #11459, .F. ) ;
#6069 = DIRECTION ( 'NONE',  ( -1.000000000000000000, 0.000000000000000000, 0.000000000000000000 ) ) ;
#6070 = VERTEX_POINT ( 'NONE', #4930 ) ;
#6071 = CARTESIAN_POINT ( 'NONE',  ( -10.00000000000000000, 0.000000000000000000, 0.000000000000000000 ) ) ;
#6072 = DIRECTION ( 'NONE',  ( -1.000000000000000000, -0.000000000000000000, 0.000000000000000000 ) ) ;
#6073 = CARTESIAN_POINT ( 'NONE',  ( 8.329772390959204742, 2.373743296044067641, 10.00000000000000000 ) ) ;
#6074 = AXIS2_PLACEMENT_3D ( 'NONE', #10971, #8096, #2341 ) ;
#6075 = CARTESIAN_POINT ( 'NONE',  ( 3.000000000000000888, 19.74380051311539930, 11.79560690673879186 ) ) ;
#6076 = CIRCLE ( 'NONE', #2357, 24.80000000000000071 ) ;
#6077 = CARTESIAN_POINT ( 'NONE',  ( 13.24268851590353790, -2.403973981684889072, 3.747395293195558847E-16 ) ) ;
#6078 = AXIS2_PLACEMENT_3D ( 'NONE', #8455, #53, #3801 ) ;
#6079 = LINE ( 'NONE', #629, #3139 ) ;
#6080 = EDGE_CURVE ( 'NONE', #1468, #10781, #5233, .T. ) ;
#6081 = CARTESIAN_POINT ( 'NONE',  ( 3.000000000000000888, 24.75110766671652129, 1.556492618230723046 ) ) ;
#6082 = EDGE_LOOP ( 'NONE', ( #10275, #4625, #2583, #919 ) ) ;
#6083 = ADVANCED_FACE ( 'NONE', ( #7553 ), #5663, .T. ) ;
#6084 = CIRCLE ( 'NONE', #2964, 1.500000000000000222 ) ;
#6085 = CARTESIAN_POINT ( 'NONE',  ( 0.000000000000000000, 24.75110766671652129, 1.556492618230723046 ) ) ;
#6086 = ORIENTED_EDGE ( 'NONE', *, *, #7020, .T. ) ;
#6087 = CIRCLE ( 'NONE', #6078, 22.99899999999999523 ) ;
#6088 = AXIS2_PLACEMENT_3D ( 'NONE', #6890, #5980, #7930 ) ;
#6089 = DIRECTION ( 'NONE',  ( 1.000000000000000000, 0.000000000000000000, -0.000000000000000000 ) ) ;
#6090 = FACE_OUTER_BOUND ( 'NONE', #10844, .T. ) ;
#6091 = CARTESIAN_POINT ( 'NONE',  ( -4.263796145714478847, -6.152586724582791433, 10.00000000000000000 ) ) ;
#6092 = CARTESIAN_POINT ( 'NONE',  ( -9.023584016175915323, 3.917288190900554579, 6.857782953271941950E-17 ) ) ;
#6093 = CYLINDRICAL_SURFACE ( 'NONE', #1990, 22.99899999999999878 ) ;
#6094 = AXIS2_PLACEMENT_3D ( 'NONE', #3637, #2655, #2715 ) ;
#6095 = DIRECTION ( 'NONE',  ( 0.000000000000000000, 0.000000000000000000, 1.000000000000000000 ) ) ;
#6096 = VERTEX_POINT ( 'NONE', #7495 ) ;
#6097 = ORIENTED_EDGE ( 'NONE', *, *, #10200, .T. ) ;
#6098 = ORIENTED_EDGE ( 'NONE', *, *, #837, .T. ) ;
#6099 = ADVANCED_FACE ( 'NONE', ( #201 ), #1927, .T. ) ;
#6100 = DIRECTION ( 'NONE',  ( 0.000000000000000000, 0.8090169943749445647, 0.5877852522924771339 ) ) ;
#6101 = STYLED_ITEM ( 'NONE', ( #3159 ), #483 ) ;
#6102 = AXIS2_PLACEMENT_3D ( 'NONE', #6241, #3369, #10834 ) ;
#6103 = CARTESIAN_POINT ( 'NONE',  ( 3.000000000000000888, 5.117118920208487687, 22.42251312757881365 ) ) ;
#6104 = CARTESIAN_POINT ( 'NONE',  ( 3.000000000000000888, -11.02759168516760369, 22.21333432029560484 ) ) ;
#6105 = EDGE_CURVE ( 'NONE', #3455, #12008, #25, .T. ) ;
#6106 = CARTESIAN_POINT ( 'NONE',  ( -2.196651480121880162, 8.111327970581170277, 3.747395293195558847E-16 ) ) ;
#6107 = DIRECTION ( 'NONE',  ( 1.000000000000000000, 0.000000000000000000, 0.000000000000000000 ) ) ;
#6108 = LINE ( 'NONE', #11555, #8797 ) ;
#6109 = EDGE_LOOP ( 'NONE', ( #980, #1675, #10154, #3770 ) ) ;
#6110 = STYLED_ITEM ( 'NONE', ( #8104 ), #6320 ) ;
#6111 = ORIENTED_EDGE ( 'NONE', *, *, #7915, .T. ) ;
#6112 = APPLICATION_PROTOCOL_DEFINITION ( 'draft international standard', 'automotive_design', 1998, #5124 ) ;
#6113 = CARTESIAN_POINT ( 'NONE',  ( -13.04979933117209967, -0.2127334381860513379, 10.00000000000000000 ) ) ;
#6114 = ORIENTED_EDGE ( 'NONE', *, *, #3559, .T. ) ;
#6115 = DIRECTION ( 'NONE',  ( 0.000000000000000000, 0.000000000000000000, 1.000000000000000000 ) ) ;
#6116 = CARTESIAN_POINT ( 'NONE',  ( -22.00000000000000000, 0.000000000000000000, 0.000000000000000000 ) ) ;
#6117 = CARTESIAN_POINT ( 'NONE',  ( 0.000000000000000000, 21.76479567747252020, -7.432877647174977120 ) ) ;
#6118 = CARTESIAN_POINT ( 'NONE',  ( 3.000000000000000888, 0.000000000000000000, 0.000000000000000000 ) ) ;
#6119 = EDGE_LOOP ( 'NONE', ( #10049, #5116, #867, #11036, #4200, #2228, #9790, #8692, #728, #6228, #1535, #11826, #9854, #9124, #11247, #660, #8525, #12020, #8064, #2663, #1771, #2696, #9172, #717, #10472, #5443, #10032, #7332, #7180, #6409, #6163, #11270, #615, #7306, #1926, #11850, #10190, #6647, #7078, #10771, #8878, #6136, #4701, #11262, #4773, #6938, #5455, #9104, #11881, #7297, #3716, #4, #2753, #2641, #2593, #8156, #10650, #4844, #12110, #4379, #3843, #7947, #10711, #8868, #487, #9332, #10202, #2649, #7190, #3704, #9225, #8371, #6572, #11172, #12109, #981, #7374, #5163, #3828, #4064, #5040, #492, #8723, #9454, #4160, #4028, #8262, #2116, #5508, #10276, #3668, #1060, #196, #8764, #9343, #10401, #4465, #10250, #8313, #3974, #1158, #5966, #2469, #3008, #5758, #10501, #9429, #10695, #5396, #8327, #461, #8266, #8308, #7564, #1184, #9085, #10589, #1368, #6049, #2863, #1658, #5731, #2818, #298, #4974, #3045, #11399, #8038, #2421, #382, #1443, #580, #10469, #2128, #4330, #7396, #2409, #9622, #3813, #2582, #11529, #6794, #7747, #2768, #6218, #2713, #9016, #410, #3919, #4201, #11656, #3961, #7615, #1222, #8941, #3990, #11658, #10454, #3381, #2449, #6775, #9003, #4552, #8760, #415, #11349, #5280, #3179, #7408, #6033, #11436, #11330, #1400, #6030, #4228, #3025, #5087, #6202, #1289, #9320, #12114, #168, #7551, #4178, #864, #2482, #5369, #2803, #4302, #7442, #4008, #7939, #2436, #5693, #744, #11075, #1597, #12035, #7474, #5448, #6739, #1710, #8544, #4772, #2821, #10946, #9053, #889, #1203, #5884, #2876, #11795, #4531, #9342, #4635, #3799, #9468, #3587, #3769, #10306, #1075, #10223, #8472, #6557, #9513, #5615, #7657, #6485, #1318, #1937, #9024, #5673, #10404, #6482, #775, #7563, #5446, #7164, #8387, #4764, #946, #11444, #150, #1266, #6971 ) ) ;
#6120 = AXIS2_PLACEMENT_3D ( 'NONE', #7948, #3986, #4039 ) ;
#6121 = DIRECTION ( 'NONE',  ( 1.000000000000000000, 0.000000000000000000, 0.000000000000000000 ) ) ;
#6122 = DIRECTION ( 'NONE',  ( 8.673617379884035472E-16, 1.000000000000000000, 0.000000000000000000 ) ) ;
#6123 = CARTESIAN_POINT ( 'NONE',  ( -0.1814876354083659327, -10.77628937513454943, 6.857782953271941950E-17 ) ) ;
#6124 = CIRCLE ( 'NONE', #651, 9.599999999999996092 ) ;
#6125 = MECHANICAL_DESIGN_GEOMETRIC_PRESENTATION_REPRESENTATION (  '', ( #11594 ), #5739 ) ;
#6126 = VERTEX_POINT ( 'NONE', #2053 ) ;
#6127 = DIRECTION ( 'NONE',  ( 0.000000000000000000, 0.000000000000000000, -1.000000000000000000 ) ) ;
#6128 = CARTESIAN_POINT ( 'NONE',  ( 3.000000000000000888, 7.432877647175492264, -21.76479567747234256 ) ) ;
#6129 = ORIENTED_EDGE ( 'NONE', *, *, #114, .T. ) ;
#6130 = AXIS2_PLACEMENT_3D ( 'NONE', #9352, #3850, #10213 ) ;
#6131 = EDGE_CURVE ( 'NONE', #6372, #3187, #7369, .T. ) ;
#6132 = CARTESIAN_POINT ( 'NONE',  ( 1.454091968623351550, 11.13059540125182778, 10.00000000000000000 ) ) ;
#6133 = ORIENTED_EDGE ( 'NONE', *, *, #4714, .T. ) ;
#6134 = CYLINDRICAL_SURFACE ( 'NONE', #1485, 22.99899999999999878 ) ;
#6135 = DIRECTION ( 'NONE',  ( -1.000000000000000000, 0.000000000000000000, -0.000000000000000000 ) ) ;
#6136 = ORIENTED_EDGE ( 'NONE', *, *, #6131, .F. ) ;
#6137 = EDGE_CURVE ( 'NONE', #3516, #411, #3038, .T. ) ;
#6138 = DIRECTION ( 'NONE',  ( -0.000000000000000000, -0.000000000000000000, -1.000000000000000000 ) ) ;
#6139 = DIRECTION ( 'NONE',  ( 0.000000000000000000, 0.000000000000000000, 1.000000000000000000 ) ) ;
#6140 = CARTESIAN_POINT ( 'NONE',  ( -5.965338750500730924, 7.524205049158505965, 10.00000000000000000 ) ) ;
#6141 = VECTOR ( 'NONE', #9821, 1000.000000000000000 ) ;
#6142 = FACE_OUTER_BOUND ( 'NONE', #200, .T. ) ;
#6143 = CARTESIAN_POINT ( 'NONE',  ( -11.62103867303406624, 2.700230667072888835, 3.747395293195558847E-16 ) ) ;
#6144 = EDGE_CURVE ( 'NONE', #3273, #994, #6500, .T. ) ;
#6145 = DIRECTION ( 'NONE',  ( -1.000000000000000000, -0.000000000000000000, 0.000000000000000000 ) ) ;
#6146 = DIRECTION ( 'NONE',  ( 0.000000000000000000, 0.000000000000000000, 1.000000000000000000 ) ) ;
#6147 = EDGE_CURVE ( 'NONE', #411, #9318, #8685, .T. ) ;
#6148 = VERTEX_POINT ( 'NONE', #6575 ) ;
#6149 = EDGE_CURVE ( 'NONE', #308, #1864, #10214, .T. ) ;
#6150 = APPLICATION_CONTEXT ( 'automotive_design' ) ;
#6151 = CIRCLE ( 'NONE', #10252, 9.599999999999997868 ) ;
#6152 = DIRECTION ( 'NONE',  ( 0.000000000000000000, 0.000000000000000000, 1.000000000000000000 ) ) ;
#6153 = VERTEX_POINT ( 'NONE', #4011 ) ;
#6154 = LINE ( 'NONE', #388, #2518 ) ;
#6155 = CARTESIAN_POINT ( 'NONE',  ( 3.000000000000000888, -22.54798042742717357, -0.4575788569254196636 ) ) ;
#6156 = CARTESIAN_POINT ( 'NONE',  ( 1.499999999999999556, -22.21333432029556576, -11.02759168516767296 ) ) ;
#6157 = CARTESIAN_POINT ( 'NONE',  ( 7.737545192982509867, 9.111483571581276308, 6.857782953271941950E-17 ) ) ;
#6158 = CARTESIAN_POINT ( 'NONE',  ( 0.000000000000000000, 24.02068490260612776, 6.168200451485839508 ) ) ;
#6159 = CIRCLE ( 'NONE', #3428, 9.599999999999996092 ) ;
#6160 = CARTESIAN_POINT ( 'NONE',  ( 1.500000000000000444, 15.80756504416717334, -19.10918332567941036 ) ) ;
#6161 = ORIENTED_EDGE ( 'NONE', *, *, #1738, .T. ) ;
#6162 = ORIENTED_EDGE ( 'NONE', *, *, #5237, .T. ) ;
#6163 = ORIENTED_EDGE ( 'NONE', *, *, #7152, .F. ) ;
#6164 = CARTESIAN_POINT ( 'NONE',  ( 0.4634152073531427884, 14.27464310366533695, 10.00000000000000000 ) ) ;
#6165 = DIRECTION ( 'NONE',  ( -1.000000000000000000, -0.000000000000000000, 0.000000000000000000 ) ) ;
#6166 = DIRECTION ( 'NONE',  ( -1.000000000000000000, -0.000000000000000000, -0.000000000000000000 ) ) ;
#6167 = CARTESIAN_POINT ( 'NONE',  ( -2.296015608618632076, -6.188270089871726221, 3.747395293195558847E-16 ) ) ;
#6168 = EDGE_CURVE ( 'NONE', #10871, #474, #5526, .T. ) ;
#6169 = DIRECTION ( 'NONE',  ( 0.000000000000000000, 0.6691306063588594588, -0.7431448254773932449 ) ) ;
#6170 = DIRECTION ( 'NONE',  ( 1.000000000000000000, -0.000000000000000000, -0.000000000000000000 ) ) ;
#6171 = ORIENTED_EDGE ( 'NONE', *, *, #7697, .F. ) ;
#6172 = ORIENTED_EDGE ( 'NONE', *, *, #2996, .F. ) ;
#6173 = AXIS2_PLACEMENT_3D ( 'NONE', #7539, #4914, #1116 ) ;
#6174 = CARTESIAN_POINT ( 'NONE',  ( -9.546882484473293573, 8.373557015401750903, 10.00000000000000000 ) ) ;
#6175 = ORIENTED_EDGE ( 'NONE', *, *, #12012, .T. ) ;
#6176 = CARTESIAN_POINT ( 'NONE',  ( -2.214925388402925410, 4.996014981202114846, 10.00000000000000000 ) ) ;
#6177 = DIRECTION ( 'NONE',  ( 0.000000000000000000, -0.8660254037844432595, 0.4999999999999919509 ) ) ;
#6178 = CARTESIAN_POINT ( 'NONE',  ( 5.000000000000000000, 6.123233995736766282E-16, 0.000000000000000000 ) ) ;
#6179 = EDGE_CURVE ( 'NONE', #2929, #8071, #10935, .T. ) ;
#6180 = DIRECTION ( 'NONE',  ( 0.000000000000000000, 0.000000000000000000, 1.000000000000000000 ) ) ;
#6181 = EDGE_LOOP ( 'NONE', ( #2823, #11437, #4891, #7519 ) ) ;
#6182 = CYLINDRICAL_SURFACE ( 'NONE', #4567, 9.599999999999997868 ) ;
#6183 = VECTOR ( 'NONE', #5892, 1000.000000000000000 ) ;
#6184 = DIRECTION ( 'NONE',  ( 0.000000000000000000, 0.000000000000000000, 1.000000000000000000 ) ) ;
#6185 = CARTESIAN_POINT ( 'NONE',  ( 9.623984404417814886, 6.889883918979093025, 6.857782953271941950E-17 ) ) ;
#6186 = DIRECTION ( 'NONE',  ( -1.000000000000000000, 0.000000000000000000, 0.000000000000000000 ) ) ;
#6187 = ORIENTED_EDGE ( 'NONE', *, *, #9356, .F. ) ;
#6188 = DIRECTION ( 'NONE',  ( 0.000000000000000000, 0.000000000000000000, 1.000000000000000000 ) ) ;
#6189 = VERTEX_POINT ( 'NONE', #10308 ) ;
#6190 = VECTOR ( 'NONE', #5447, 1000.000000000000000 ) ;
#6191 = CARTESIAN_POINT ( 'NONE',  ( 7.316052646047090491, -7.060001943526881263, 10.00000000000000000 ) ) ;
#6192 = ORIENTED_EDGE ( 'NONE', *, *, #7632, .F. ) ;
#6193 = CARTESIAN_POINT ( 'NONE',  ( 3.000000000000000888, 9.039786367039127413, -21.14796121233187520 ) ) ;
#6194 = CARTESIAN_POINT ( 'NONE',  ( 3.000000000000000888, 24.53384959170457691, 3.623565124517186931 ) ) ;
#6195 = CARTESIAN_POINT ( 'NONE',  ( -3.000000000000000000, 3.673940397442059868E-16, 10.00000000000000000 ) ) ;
#6196 = DIRECTION ( 'NONE',  ( -1.000000000000000000, -0.000000000000000000, 0.000000000000000000 ) ) ;
#6197 = CARTESIAN_POINT ( 'NONE',  ( 7.763517025773944980, -3.069710483245354116, 10.00000000000000000 ) ) ;
#6198 = CARTESIAN_POINT ( 'NONE',  ( 3.000000000000000888, -11.67026512804534022, -19.29833442572371638 ) ) ;
#6199 = CARTESIAN_POINT ( 'NONE',  ( 4.977139221860116258, 13.21892491369776934, 3.747395293195558847E-16 ) ) ;
#6200 = CARTESIAN_POINT ( 'NONE',  ( 0.000000000000000000, 17.35216073792464897, -17.71842311621511712 ) ) ;
#6201 = DIRECTION ( 'NONE',  ( -1.000000000000000000, -0.000000000000000000, 0.000000000000000000 ) ) ;
#6202 = ORIENTED_EDGE ( 'NONE', *, *, #2324, .F. ) ;
#6203 = DIRECTION ( 'NONE',  ( 0.000000000000000000, 0.000000000000000000, -1.000000000000000000 ) ) ;
#6204 = DIRECTION ( 'NONE',  ( 0.000000000000000000, 0.000000000000000000, 1.000000000000000000 ) ) ;
#6205 = FILL_AREA_STYLE ('',( #7350 ) ) ;
#6206 = ORIENTED_EDGE ( 'NONE', *, *, #633, .T. ) ;
#6207 = CYLINDRICAL_SURFACE ( 'NONE', #5036, 11.50000000000000178 ) ;
#6208 = EDGE_CURVE ( 'NONE', #6263, #7573, #11294, .T. ) ;
#6209 = DIRECTION ( 'NONE',  ( 0.000000000000000000, 0.000000000000000000, 1.000000000000000000 ) ) ;
#6210 = CARTESIAN_POINT ( 'NONE',  ( 1.499999999999999556, 6.168200451486086422, -24.02068490260606026 ) ) ;
#6211 = CARTESIAN_POINT ( 'NONE',  ( 9.623984404417814886, 6.889883918979093025, 6.857782953271941950E-17 ) ) ;
#6212 = DIRECTION ( 'NONE',  ( -1.000000000000000000, -0.000000000000000000, -0.000000000000000000 ) ) ;
#6213 = EDGE_CURVE ( 'NONE', #6294, #10654, #10155, .T. ) ;
#6214 = DIRECTION ( 'NONE',  ( -1.000000000000000000, 0.000000000000000000, -0.000000000000000000 ) ) ;
#6215 = ORIENTED_EDGE ( 'NONE', *, *, #8864, .T. ) ;
#6216 = CIRCLE ( 'NONE', #6978, 9.599999999999997868 ) ;
#6217 = ORIENTED_EDGE ( 'NONE', *, *, #1389, .F. ) ;
#6218 = ORIENTED_EDGE ( 'NONE', *, *, #10692, .F. ) ;
#6219 = CARTESIAN_POINT ( 'NONE',  ( -10.73274959028002229, -5.974010873319484105, 10.00000000000000000 ) ) ;
#6220 = ADVANCED_FACE ( 'NONE', ( #2911 ), #6633, .T. ) ;
#6221 = CARTESIAN_POINT ( 'NONE',  ( 3.000000000000000888, -2.062268319295407881, -22.90635393027948297 ) ) ;
#6222 = CARTESIAN_POINT ( 'NONE',  ( 3.000000000000000888, 22.56530478845654386, -4.445336973060635799 ) ) ;
#6223 = AXIS2_PLACEMENT_3D ( 'NONE', #5863, #1270, #11610 ) ;
#6224 = CIRCLE ( 'NONE', #11694, 24.80000000000000071 ) ;
#6225 = CARTESIAN_POINT ( 'NONE',  ( -6.012500708481076650, 0.06204199954272016787, 3.747395293195558847E-16 ) ) ;
#6226 = DIRECTION ( 'NONE',  ( -1.000000000000000000, 0.000000000000000000, 0.000000000000000000 ) ) ;
#6227 = CARTESIAN_POINT ( 'NONE',  ( 3.000000000000000888, 22.83456483164689033, 2.745295967526073078 ) ) ;
#6228 = ORIENTED_EDGE ( 'NONE', *, *, #11956, .F. ) ;
#6229 = ORIENTED_EDGE ( 'NONE', *, *, #7399, .F. ) ;
#6230 = EDGE_CURVE ( 'NONE', #3076, #8331, #2063, .T. ) ;
#6231 = EDGE_LOOP ( 'NONE', ( #86, #2936, #2985, #10305 ) ) ;
#6232 = CARTESIAN_POINT ( 'NONE',  ( 0.8073695008816145213, 5.181225205791319510, 10.00000000000000000 ) ) ;
#6233 = VECTOR ( 'NONE', #11054, 1000.000000000000000 ) ;
#6234 = AXIS2_PLACEMENT_3D ( 'NONE', #6025, #9752, #2411 ) ;
#6235 = FACE_BOUND ( 'NONE', #10567, .T. ) ;
#6236 = DIRECTION ( 'NONE',  ( 0.000000000000000000, -0.3090169943749349057, -0.9510565162951577500 ) ) ;
#6237 = EDGE_CURVE ( 'NONE', #8914, #363, #4866, .T. ) ;
#6238 = FACE_OUTER_BOUND ( 'NONE', #5729, .T. ) ;
#6239 = ORIENTED_EDGE ( 'NONE', *, *, #12044, .F. ) ;
#6240 = DIRECTION ( 'NONE',  ( -1.000000000000000000, 0.000000000000000000, 0.000000000000000000 ) ) ;
#6241 = CARTESIAN_POINT ( 'NONE',  ( 3.000000000000000888, 0.000000000000000000, 0.000000000000000000 ) ) ;
#6242 = CARTESIAN_POINT ( 'NONE',  ( 3.343943643650757913, -10.41127694127634129, 6.857782953271941950E-17 ) ) ;
#6243 = COLOUR_RGB ( '', 0.72549020, 0.75294118, 0.79215686) ;
#6244 = ADVANCED_FACE ( 'NONE', ( #8726 ), #4067, .T. ) ;
#6245 = DIRECTION ( 'NONE',  ( 0.000000000000000000, 0.000000000000000000, 1.000000000000000000 ) ) ;
#6246 = DIRECTION ( 'NONE',  ( -1.000000000000000000, -0.000000000000000000, -0.000000000000000000 ) ) ;
#6247 = ORIENTED_EDGE ( 'NONE', *, *, #11476, .F. ) ;
#6248 = VERTEX_POINT ( 'NONE', #4989 ) ;
#6249 = CARTESIAN_POINT ( 'NONE',  ( -4.158472309566741743, 3.840014155104743754, 10.00000000000000000 ) ) ;
#6250 = CIRCLE ( 'NONE', #4286, 19.99999999999999645 ) ;
#6251 = ORIENTED_EDGE ( 'NONE', *, *, #7802, .T. ) ;
#6252 = CARTESIAN_POINT ( 'NONE',  ( 0.000000000000000000, 24.77821629063821973, 1.039229259764575364 ) ) ;
#6253 = CIRCLE ( 'NONE', #2335, 4.000000000000000000 ) ;
#6254 = CARTESIAN_POINT ( 'NONE',  ( 3.000000000000000888, 8.753070780933159156, 20.78471918669863427 ) ) ;
#6255 = DIRECTION ( 'NONE',  ( 0.000000000000000000, 0.2079116908177598144, -0.9781476007338055778 ) ) ;
#6256 = CARTESIAN_POINT ( 'NONE',  ( -9.977213461302319786, -1.645879626164742593, 10.00000000000000000 ) ) ;
#6257 = FACE_OUTER_BOUND ( 'NONE', #1350, .T. ) ;
#6258 = EDGE_CURVE ( 'NONE', #10654, #6294, #1476, .T. ) ;
#6259 = DIRECTION ( 'NONE',  ( -1.000000000000000000, 0.000000000000000000, 0.000000000000000000 ) ) ;
#6260 = VERTEX_POINT ( 'NONE', #328 ) ;
#6261 = CARTESIAN_POINT ( 'NONE',  ( -22.00000000000000000, 0.000000000000000000, 0.000000000000000000 ) ) ;
#6262 = VECTOR ( 'NONE', #8123, 1000.000000000000000 ) ;
#6263 = VERTEX_POINT ( 'NONE', #4132 ) ;
#6264 = CARTESIAN_POINT ( 'NONE',  ( 3.194803811556592876, -2.743189786380903161, 3.747395293195558847E-16 ) ) ;
#6265 = DIRECTION ( 'NONE',  ( 0.000000000000000000, 0.000000000000000000, 1.000000000000000000 ) ) ;
#6266 = EDGE_LOOP ( 'NONE', ( #9223, #7299, #10036, #6599 ) ) ;
#6267 = AXIS2_PLACEMENT_3D ( 'NONE', #4418, #9015, #1426 ) ;
#6268 = DIRECTION ( 'NONE',  ( -1.000000000000000000, 0.000000000000000000, 0.000000000000000000 ) ) ;
#6269 = VECTOR ( 'NONE', #9115, 1000.000000000000000 ) ;
#6270 = AXIS2_PLACEMENT_3D ( 'NONE', #9132, #4479, #1428 ) ;
#6271 = CARTESIAN_POINT ( 'NONE',  ( 1.500000000000000444, -19.10918332567947076, -15.80756504416710229 ) ) ;
#6272 = CARTESIAN_POINT ( 'NONE',  ( -2.100379401128186441, -7.348625593045292170, 10.00000000000000000 ) ) ;
#6273 = CARTESIAN_POINT ( 'NONE',  ( 10.54603994011982415, 5.199563424939647405, 6.857782953271941950E-17 ) ) ;
#6274 = MECHANICAL_DESIGN_GEOMETRIC_PRESENTATION_REPRESENTATION (  '', ( #4124 ), #10963 ) ;
#6275 = DIRECTION ( 'NONE',  ( -1.000000000000000000, -0.000000000000000000, -0.000000000000000000 ) ) ;
#6276 = CARTESIAN_POINT ( 'NONE',  ( 3.000000000000000888, 22.54798042742718067, -0.4575788569252652871 ) ) ;
#6277 = VERTEX_POINT ( 'NONE', #6085 ) ;
#6278 = AXIS2_PLACEMENT_3D ( 'NONE', #4971, #8707, #1290 ) ;
#6279 = ORIENTED_EDGE ( 'NONE', *, *, #4263, .T. ) ;
#6280 = ADVANCED_FACE ( 'NONE', ( #450 ), #4243, .T. ) ;
#6281 = AXIS2_PLACEMENT_3D ( 'NONE', #7658, #3495, #5205 ) ;
#6282 = ORIENTED_EDGE ( 'NONE', *, *, #2461, .T. ) ;
#6283 = CARTESIAN_POINT ( 'NONE',  ( -11.08238827499401680, -10.71925978067563001, 10.00000000000000000 ) ) ;
#6284 = EDGE_CURVE ( 'NONE', #3450, #7701, #7797, .T. ) ;
#6285 = CARTESIAN_POINT ( 'NONE',  ( 0.000000000000000000, 19.75591328264900781, -10.87771529938142123 ) ) ;
#6286 = CYLINDRICAL_SURFACE ( 'NONE', #3301, 9.599999999999997868 ) ;
#6287 = CARTESIAN_POINT ( 'NONE',  ( 0.000000000000000000, 0.000000000000000000, 0.000000000000000000 ) ) ;
#6288 = EDGE_CURVE ( 'NONE', #8212, #9360, #8323, .T. ) ;
#6289 = CIRCLE ( 'NONE', #3349, 24.80000000000000071 ) ;
#6290 = CARTESIAN_POINT ( 'NONE',  ( -4.491015865170908228, 3.510096388331549910, 3.747395293195558847E-16 ) ) ;
#6291 = FACE_OUTER_BOUND ( 'NONE', #7656, .T. ) ;
#6292 = EDGE_CURVE ( 'NONE', #2317, #10809, #691, .T. ) ;
#6293 = DIRECTION ( 'NONE',  ( 0.000000000000000000, -0.9510565162951566398, 0.3090169943749382919 ) ) ;
#6294 = VERTEX_POINT ( 'NONE', #9750 ) ;
#6295 = ORIENTED_EDGE ( 'NONE', *, *, #5274, .T. ) ;
#6296 = CONTEXT_DEPENDENT_SHAPE_REPRESENTATION ( #8420, #5904 ) ;
#6297 = EDGE_CURVE ( 'NONE', #4270, #9364, #10866, .T. ) ;
#6298 = AXIS2_PLACEMENT_3D ( 'NONE', #5783, #9506, #378 ) ;
#6299 = ORIENTED_EDGE ( 'NONE', *, *, #8120, .F. ) ;
#6300 = DIRECTION ( 'NONE',  ( -1.000000000000000000, 0.000000000000000000, 0.000000000000000000 ) ) ;
#6301 = VECTOR ( 'NONE', #6731, 1000.000000000000000 ) ;
#6302 = DIRECTION ( 'NONE',  ( 1.000000000000000000, -0.000000000000000000, -0.000000000000000000 ) ) ;
#6303 = LINE ( 'NONE', #9052, #2279 ) ;
#6304 = VERTEX_POINT ( 'NONE', #3212 ) ;
#6305 = CARTESIAN_POINT ( 'NONE',  ( 0.000000000000000000, 8.645255683529311952, -23.24434456306316577 ) ) ;
#6306 = FACE_OUTER_BOUND ( 'NONE', #636, .T. ) ;
#6307 = CARTESIAN_POINT ( 'NONE',  ( 0.0002901587068756704066, -4.749354241797638210, 6.857782953271941950E-17 ) ) ;
#6308 = CIRCLE ( 'NONE', #2785, 9.599999999999997868 ) ;
#6309 = DIRECTION ( 'NONE',  ( 0.000000000000000000, 0.000000000000000000, 1.000000000000000000 ) ) ;
#6310 = DIRECTION ( 'NONE',  ( 0.000000000000000000, -0.5877852522924797984, 0.8090169943749426773 ) ) ;
#6311 = VERTEX_POINT ( 'NONE', #6930 ) ;
#6312 = CYLINDRICAL_SURFACE ( 'NONE', #9, 24.80000000000000071 ) ;
#6313 = EDGE_LOOP ( 'NONE', ( #6718, #10961, #8856, #6774 ) ) ;
#6314 = CARTESIAN_POINT ( 'NONE',  ( -3.231136241382285501, -5.666136714101813965, 10.00000000000000000 ) ) ;
#6315 = SHAPE_REPRESENTATION ( 'cap', ( #8474 ), #4902 ) ;
#6316 =( GEOMETRIC_REPRESENTATION_CONTEXT ( 3 ) GLOBAL_UNCERTAINTY_ASSIGNED_CONTEXT ( ( #9293 ) ) GLOBAL_UNIT_ASSIGNED_CONTEXT ( ( #5409, #568, #3459 ) ) REPRESENTATION_CONTEXT ( 'NONE', 'WORKASPACE' ) );
#6317 = ORIENTED_EDGE ( 'NONE', *, *, #2282, .F. ) ;
#6318 = DIRECTION ( 'NONE',  ( -1.000000000000000000, -0.000000000000000000, -0.000000000000000000 ) ) ;
#6319 = ORIENTED_EDGE ( 'NONE', *, *, #6602, .F. ) ;
#6320 = ADVANCED_BREP_SHAPE_REPRESENTATION ( '', ( #8430, #8474 ), #5529 ) ;
#6321 = CARTESIAN_POINT ( 'NONE',  ( 0.000000000000000000, 9.128825345753028842, 23.05871956130125611 ) ) ;
#6322 = CIRCLE ( 'NONE', #6703, 22.99900000000000233 ) ;
#6323 = CYLINDRICAL_SURFACE ( 'NONE', #12010, 9.599999999999997868 ) ;
#6324 = CARTESIAN_POINT ( 'NONE',  ( -11.80455809908225717, -11.41585333555581627, 6.857782953271941950E-17 ) ) ;
#6325 = EDGE_CURVE ( 'NONE', #6367, #110, #11252, .T. ) ;
#6326 = CYLINDRICAL_SURFACE ( 'NONE', #5298, 22.99899999999999878 ) ;
#6327 = AXIS2_PLACEMENT_3D ( 'NONE', #9072, #683, #10965 ) ;
#6328 = ORIENTED_EDGE ( 'NONE', *, *, #6655, .F. ) ;
#6329 = DIRECTION ( 'NONE',  ( 0.000000000000000000, -0.6691306063588644548, 0.7431448254773885820 ) ) ;
#6330 = ORIENTED_EDGE ( 'NONE', *, *, #6755, .T. ) ;
#6331 = CARTESIAN_POINT ( 'NONE',  ( 3.678979105947487671, -2.215585777442455662, 3.747395293195558847E-16 ) ) ;
#6332 = CARTESIAN_POINT ( 'NONE',  ( -2.958039891549808509, 0.5000000000000001110, 3.000000000000000000 ) ) ;
#6333 = SURFACE_SIDE_STYLE ('',( #7167 ) ) ;
#6334 = VERTEX_POINT ( 'NONE', #5967 ) ;
#6335 = EDGE_CURVE ( 'NONE', #11607, #8421, #10072, .T. ) ;
#6336 = CIRCLE ( 'NONE', #1057, 9.599999999999997868 ) ;
#6337 = DIRECTION ( 'NONE',  ( -1.000000000000000000, 0.000000000000000000, -0.000000000000000000 ) ) ;
#6338 = FACE_OUTER_BOUND ( 'NONE', #4501, .T. ) ;
#6339 = DIRECTION ( 'NONE',  ( -1.000000000000000000, -0.000000000000000000, 0.000000000000000000 ) ) ;
#6340 = CARTESIAN_POINT ( 'NONE',  ( 7.763517025772753044, -3.069710483245351451, 6.857782953271941950E-17 ) ) ;
#6341 = LINE ( 'NONE', #7176, #10221 ) ;
#6342 = FACE_OUTER_BOUND ( 'NONE', #480, .T. ) ;
#6343 = ORIENTED_EDGE ( 'NONE', *, *, #10122, .T. ) ;
#6344 = ORIENTED_EDGE ( 'NONE', *, *, #6395, .F. ) ;
#6345 = AXIS2_PLACEMENT_3D ( 'NONE', #11099, #10916, #9028 ) ;
#6346 = ORIENTED_EDGE ( 'NONE', *, *, #7399, .T. ) ;
#6347 = CARTESIAN_POINT ( 'NONE',  ( -14.85975435031504865, 1.953672781916663936, 10.00000000000000000 ) ) ;
#6348 = CARTESIAN_POINT ( 'NONE',  ( 0.000000000000000000, -22.99643626497956461, -0.3433949777334098785 ) ) ;
#6349 = DIRECTION ( 'NONE',  ( -1.000000000000000000, -0.000000000000000000, -0.000000000000000000 ) ) ;
#6350 = CARTESIAN_POINT ( 'NONE',  ( 3.120778274233606098, -6.257845451233481349, 3.747395293195558847E-16 ) ) ;
#6351 = CARTESIAN_POINT ( 'NONE',  ( 0.000000000000000000, 22.47229024614980020, -1.901833551798019162 ) ) ;
#6352 = EDGE_LOOP ( 'NONE', ( #3499, #8033, #5586, #9774 ) ) ;
#6353 = FACE_OUTER_BOUND ( 'NONE', #3733, .T. ) ;
#6354 = VERTEX_POINT ( 'NONE', #10860 ) ;
#6355 = ORIENTED_EDGE ( 'NONE', *, *, #32, .F. ) ;
#6356 = CARTESIAN_POINT ( 'NONE',  ( 2.084958754360777711, -3.480815169282206689, 10.00000000000000000 ) ) ;
#6357 = EDGE_CURVE ( 'NONE', #1474, #3450, #8901, .T. ) ;
#6358 = DIRECTION ( 'NONE',  ( -1.000000000000000000, 0.000000000000000000, 0.000000000000000000 ) ) ;
#6359 = CARTESIAN_POINT ( 'NONE',  ( -10.00000000000000000, 0.000000000000000000, 0.000000000000000000 ) ) ;
#6360 = DIRECTION ( 'NONE',  ( 0.000000000000000000, 0.000000000000000000, -1.000000000000000000 ) ) ;
#6361 = ADVANCED_FACE ( 'NONE', ( #1370 ), #7916, .T. ) ;
#6362 = DIRECTION ( 'NONE',  ( -1.000000000000000000, -0.000000000000000000, 0.000000000000000000 ) ) ;
#6363 = CARTESIAN_POINT ( 'NONE',  ( 5.267519402444978738, 2.381954139586884622, 6.857782953271941950E-17 ) ) ;
#6364 = CIRCLE ( 'NONE', #11055, 24.80000000000000071 ) ;
#6365 = ADVANCED_FACE ( 'NONE', ( #4190 ), #6986, .T. ) ;
#6366 = CARTESIAN_POINT ( 'NONE',  ( 0.000000000000000000, -21.96011696265495061, 5.135568396239952982 ) ) ;
#6367 = VERTEX_POINT ( 'NONE', #567 ) ;
#6368 = DIRECTION ( 'NONE',  ( -1.000000000000000000, 0.000000000000000000, 0.000000000000000000 ) ) ;
#6369 = VERTEX_POINT ( 'NONE', #5045 ) ;
#6370 = EDGE_LOOP ( 'NONE', ( #3411, #6998, #6002, #4469 ) ) ;
#6371 = CARTESIAN_POINT ( 'NONE',  ( 2.467392210070201486, 7.745125807189176648, 10.00000000000000000 ) ) ;
#6372 = VERTEX_POINT ( 'NONE', #4301 ) ;
#6373 = CARTESIAN_POINT ( 'NONE',  ( 3.000000000000000888, 0.000000000000000000, 0.000000000000000000 ) ) ;
#6374 = CIRCLE ( 'NONE', #6567, 22.99900000000000233 ) ;
#6375 = ORIENTED_EDGE ( 'NONE', *, *, #2268, .T. ) ;
#6376 = CARTESIAN_POINT ( 'NONE',  ( 8.000000000000000000, 0.000000000000000000, 0.000000000000000000 ) ) ;
#6377 = CARTESIAN_POINT ( 'NONE',  ( 3.000000000000000888, -20.08719549084857192, -11.20082935824096459 ) ) ;
#6378 = CARTESIAN_POINT ( 'NONE',  ( -3.542987847618590536, 5.503081486278161627, 10.00000000000000000 ) ) ;
#6379 = DIRECTION ( 'NONE',  ( -1.000000000000000000, 0.000000000000000000, 0.000000000000000000 ) ) ;
#6380 = CARTESIAN_POINT ( 'NONE',  ( 0.000000000000000000, -16.45023496161675780, 15.42759117534379953 ) ) ;
#6381 = ORIENTED_EDGE ( 'NONE', *, *, #6237, .F. ) ;
#6382 = CARTESIAN_POINT ( 'NONE',  ( 3.000000000000000000, 0.000000000000000000, 19.99999999999999645 ) ) ;
#6383 = ORIENTED_EDGE ( 'NONE', *, *, #6728, .F. ) ;
#6384 = ADVANCED_FACE ( 'NONE', ( #8037 ), #386, .T. ) ;
#6385 = CARTESIAN_POINT ( 'NONE',  ( 7.536008357046521944, 0.2705779428718260160, 3.747395293195558847E-16 ) ) ;
#6386 = CYLINDRICAL_SURFACE ( 'NONE', #9099, 24.80000000000000071 ) ;
#6387 = ADVANCED_FACE ( 'NONE', ( #3266 ), #10732, .T. ) ;
#6388 = DIRECTION ( 'NONE',  ( 0.000000000000000000, -0.9510565162951503115, -0.3090169943749572767 ) ) ;
#6389 = DIRECTION ( 'NONE',  ( 0.000000000000000000, 0.000000000000000000, 1.000000000000000000 ) ) ;
#6390 = CARTESIAN_POINT ( 'NONE',  ( -14.19814495527487352, 7.008511237308415964, 10.00000000000000000 ) ) ;
#6391 = CARTESIAN_POINT ( 'NONE',  ( -5.248573321596925467, 4.168074790661427720, 6.857782953271941950E-17 ) ) ;
#6392 = DIRECTION ( 'NONE',  ( 0.000000000000000000, 0.000000000000000000, 1.000000000000000000 ) ) ;
#6393 = DIRECTION ( 'NONE',  ( 1.000000000000000000, 0.000000000000000000, 0.000000000000000000 ) ) ;
#6394 = EDGE_LOOP ( 'NONE', ( #6229, #8554, #11971, #1953 ) ) ;
#6395 = EDGE_CURVE ( 'NONE', #9406, #1101, #9084, .T. ) ;
#6396 = ORIENTED_EDGE ( 'NONE', *, *, #2771, .F. ) ;
#6397 = VERTEX_POINT ( 'NONE', #7166 ) ;
#6398 = CARTESIAN_POINT ( 'NONE',  ( 11.62709622633371076, -6.461356448465072511, 10.00000000000000000 ) ) ;
#6399 = CARTESIAN_POINT ( 'NONE',  ( 0.000000000000000000, 0.000000000000000000, 0.000000000000000000 ) ) ;
#6400 = DIRECTION ( 'NONE',  ( 0.000000000000000000, 0.000000000000000000, 1.000000000000000000 ) ) ;
#6401 = CARTESIAN_POINT ( 'NONE',  ( -1.719633853164446613, -9.543036404944416518, 3.747395293195558847E-16 ) ) ;
#6402 = AXIS2_PLACEMENT_3D ( 'NONE', #4020, #8680, #279 ) ;
#6403 = CARTESIAN_POINT ( 'NONE',  ( 0.000000000000000000, 0.000000000000000000, 0.000000000000000000 ) ) ;
#6404 = EDGE_CURVE ( 'NONE', #6837, #1013, #5589, .T. ) ;
#6405 = VECTOR ( 'NONE', #11638, 1000.000000000000000 ) ;
#6406 = CARTESIAN_POINT ( 'NONE',  ( 3.000000000000000888, 0.000000000000000000, 0.000000000000000000 ) ) ;
#6407 = ORIENTED_EDGE ( 'NONE', *, *, #8530, .F. ) ;
#6408 = LINE ( 'NONE', #10013, #11536 ) ;
#6409 = ORIENTED_EDGE ( 'NONE', *, *, #590, .F. ) ;
#6410 = ORIENTED_EDGE ( 'NONE', *, *, #5684, .F. ) ;
#6411 = DIRECTION ( 'NONE',  ( -1.000000000000000000, -0.000000000000000000, 0.000000000000000000 ) ) ;
#6412 = CARTESIAN_POINT ( 'NONE',  ( 0.000000000000000000, 0.000000000000000000, 0.000000000000000000 ) ) ;
#6413 = AXIS2_PLACEMENT_3D ( 'NONE', #5196, #7137, #2499 ) ;
#6414 = CARTESIAN_POINT ( 'NONE',  ( -2.958039891549808509, 0.5000000000000001110, 3.000000000000000000 ) ) ;
#6415 = DIRECTION ( 'NONE',  ( -1.000000000000000000, -0.000000000000000000, 0.000000000000000000 ) ) ;
#6416 = CARTESIAN_POINT ( 'NONE',  ( 3.000000000000000888, 0.000000000000000000, 0.000000000000000000 ) ) ;
#6417 = DIRECTION ( 'NONE',  ( -1.000000000000000000, 0.000000000000000000, 0.000000000000000000 ) ) ;
#6418 = CARTESIAN_POINT ( 'NONE',  ( 4.698850784960272087, -6.565226861933591174, 6.857782953271941950E-17 ) ) ;
#6419 = LINE ( 'NONE', #10149, #6652 ) ;
#6420 = VECTOR ( 'NONE', #954, 1000.000000000000000 ) ;
#6421 = ORIENTED_EDGE ( 'NONE', *, *, #9833, .T. ) ;
#6422 = ORIENTED_EDGE ( 'NONE', *, *, #12112, .T. ) ;
#6423 = AXIS2_PLACEMENT_3D ( 'NONE', #8548, #1022, #6635 ) ;
#6424 = LINE ( 'NONE', #1707, #2169 ) ;
#6425 = ORIENTED_EDGE ( 'NONE', *, *, #303, .T. ) ;
#6426 = ORIENTED_EDGE ( 'NONE', *, *, #5981, .T. ) ;
#6427 = CARTESIAN_POINT ( 'NONE',  ( 4.140589500486091090, -5.731468560951012314, 10.00000000000000000 ) ) ;
#6428 = ADVANCED_FACE ( 'NONE', ( #5285 ), #6386, .T. ) ;
#6429 = ORIENTED_EDGE ( 'NONE', *, *, #2304, .T. ) ;
#6430 = LINE ( 'NONE', #4468, #2659 ) ;
#6431 = EDGE_LOOP ( 'NONE', ( #3105, #3497, #5713, #1955 ) ) ;
#6432 = EDGE_CURVE ( 'NONE', #7624, #3496, #3049, .T. ) ;
#6433 = CIRCLE ( 'NONE', #3900, 24.80000000000000071 ) ;
#6434 = CARTESIAN_POINT ( 'NONE',  ( 0.000000000000000000, 21.96011696265491153, -5.135568396240103084 ) ) ;
#6435 = FACE_OUTER_BOUND ( 'NONE', #97, .T. ) ;
#6436 = CARTESIAN_POINT ( 'NONE',  ( -0.5113267480521390684, 6.289062763288780999, 10.00000000000000000 ) ) ;
#6437 = CARTESIAN_POINT ( 'NONE',  ( 3.000000000000000888, 0.000000000000000000, 0.000000000000000000 ) ) ;
#6438 = VERTEX_POINT ( 'NONE', #3693 ) ;
#6439 = CYLINDRICAL_SURFACE ( 'NONE', #8816, 24.80000000000000071 ) ;
#6440 = ORIENTED_EDGE ( 'NONE', *, *, #2347, .F. ) ;
#6441 = EDGE_CURVE ( 'NONE', #5393, #7011, #8721, .T. ) ;
#6442 = CARTESIAN_POINT ( 'NONE',  ( -2.214925388403154116, 4.996014981202573146, 3.747395293195558847E-16 ) ) ;
#6443 = ADVANCED_FACE ( 'NONE', ( #815 ), #8159, .T. ) ;
#6444 = AXIS2_PLACEMENT_3D ( 'NONE', #346, #9898, #3176 ) ;
#6445 = DIRECTION ( 'NONE',  ( -1.000000000000000000, -0.000000000000000000, -0.000000000000000000 ) ) ;
#6446 = CARTESIAN_POINT ( 'NONE',  ( 3.000000000000000888, 12.88318129270179035, 18.51065745848382349 ) ) ;
#6447 = CYLINDRICAL_SURFACE ( 'NONE', #467, 9.599999999999997868 ) ;
#6448 = DIRECTION ( 'NONE',  ( 0.000000000000000000, -0.7431448254773863615, -0.6691306063588672304 ) ) ;
#6449 = AXIS2_PLACEMENT_3D ( 'NONE', #1824, #153, #6646 ) ;
#6450 = CARTESIAN_POINT ( 'NONE',  ( 6.689389171169558779, -4.795626085247174153, 6.857782953271941950E-17 ) ) ;
#6451 = FACE_OUTER_BOUND ( 'NONE', #6727, .T. ) ;
#6452 = AXIS2_PLACEMENT_3D ( 'NONE', #7913, #2972, #1254 ) ;
#6453 = DIRECTION ( 'NONE',  ( 0.000000000000000000, 0.000000000000000000, -1.000000000000000000 ) ) ;
#6454 = ORIENTED_EDGE ( 'NONE', *, *, #9134, .F. ) ;
#6455 = EDGE_CURVE ( 'NONE', #3496, #4018, #10273, .T. ) ;
#6456 = VERTEX_POINT ( 'NONE', #2598 ) ;
#6457 = CYLINDRICAL_SURFACE ( 'NONE', #7602, 24.80000000000000071 ) ;
#6458 = CARTESIAN_POINT ( 'NONE',  ( -1.515734900794040829, 8.225284064336937817, 10.00000000000000000 ) ) ;
#6459 = DIRECTION ( 'NONE',  ( -1.000000000000000000, 0.000000000000000000, -0.000000000000000000 ) ) ;
#6460 = DIRECTION ( 'NONE',  ( -1.000000000000000000, 0.000000000000000000, 0.000000000000000000 ) ) ;
#6461 = PRODUCT_DEFINITION_FORMATION_WITH_SPECIFIED_SOURCE ( 'ANY', '', #220, .NOT_KNOWN. ) ;
#6462 = CARTESIAN_POINT ( 'NONE',  ( 3.053028024665286111, -9.450988318041344982, 3.747395293195558847E-16 ) ) ;
#6463 = CARTESIAN_POINT ( 'NONE',  ( 4.340769014460001962, -0.9713985772308075806, 3.747395293195558847E-16 ) ) ;
#6464 = CYLINDRICAL_SURFACE ( 'NONE', #611, 9.599999999999997868 ) ;
#6465 = EDGE_CURVE ( 'NONE', #10686, #2021, #11041, .T. ) ;
#6466 = VERTEX_POINT ( 'NONE', #11886 ) ;
#6467 = ORIENTED_EDGE ( 'NONE', *, *, #6687, .T. ) ;
#6468 = ORIENTED_EDGE ( 'NONE', *, *, #1127, .F. ) ;
#6469 = DIRECTION ( 'NONE',  ( -1.000000000000000000, 0.000000000000000000, 0.000000000000000000 ) ) ;
#6470 = CARTESIAN_POINT ( 'NONE',  ( 3.000000000000000888, 22.99643626497956816, -0.3433949777332470088 ) ) ;
#6471 = AXIS2_PLACEMENT_3D ( 'NONE', #952, #3709, #2855 ) ;
#6472 = AXIS2_PLACEMENT_3D ( 'NONE', #1509, #588, #4325 ) ;
#6473 = CARTESIAN_POINT ( 'NONE',  ( 0.000000000000000000, -7.432877647175354596, 21.76479567747239230 ) ) ;
#6474 = DIRECTION ( 'NONE',  ( 0.000000000000000000, 0.000000000000000000, 1.000000000000000000 ) ) ;
#6475 = EDGE_CURVE ( 'NONE', #8517, #6311, #3515, .T. ) ;
#6476 = CARTESIAN_POINT ( 'NONE',  ( 3.000000000000000888, 1.556492618230640002, 24.75110766671652840 ) ) ;
#6477 = CARTESIAN_POINT ( 'NONE',  ( 13.54728169684850059, 0.8932250400879224728, 3.747395293195558847E-16 ) ) ;
#6478 = CARTESIAN_POINT ( 'NONE',  ( -1.032305814202111760, 6.265050879046235366, 6.857782953271941950E-17 ) ) ;
#6479 = CIRCLE ( 'NONE', #6298, 9.599999999999996092 ) ;
#6480 = CARTESIAN_POINT ( 'NONE',  ( 0.000000000000000000, 0.000000000000000000, 0.000000000000000000 ) ) ;
#6481 = ORIENTED_EDGE ( 'NONE', *, *, #596, .T. ) ;
#6482 = ORIENTED_EDGE ( 'NONE', *, *, #3518, .F. ) ;
#6483 = CARTESIAN_POINT ( 'NONE',  ( 3.000000000000000888, 0.000000000000000000, 0.000000000000000000 ) ) ;
#6484 = VECTOR ( 'NONE', #11748, 1000.000000000000000 ) ;
#6485 = ORIENTED_EDGE ( 'NONE', *, *, #2477, .F. ) ;
#6486 = ORIENTED_EDGE ( 'NONE', *, *, #143, .T. ) ;
#6487 = CARTESIAN_POINT ( 'NONE',  ( 0.07364157424580680678, -3.751631698233684364, 10.00000000000000000 ) ) ;
#6488 = CARTESIAN_POINT ( 'NONE',  ( 0.000000000000000000, 0.000000000000000000, 3.000000000000000000 ) ) ;
#6489 = VERTEX_POINT ( 'NONE', #5464 ) ;
#6490 = AXIS2_PLACEMENT_3D ( 'NONE', #10527, #10751, #3989 ) ;
#6491 = AXIS2_PLACEMENT_3D ( 'NONE', #8640, #1407, #9672 ) ;
#6492 = DIRECTION ( 'NONE',  ( 0.000000000000000000, 0.9945218953682736229, -0.1045284632676503622 ) ) ;
#6493 = CARTESIAN_POINT ( 'NONE',  ( 0.000000000000000000, 2.811977935937781670, 22.37663021667345120 ) ) ;
#6494 = CARTESIAN_POINT ( 'NONE',  ( -3.791520748785365491, -16.26028641251512497, 6.857782953271941950E-17 ) ) ;
#6495 = CARTESIAN_POINT ( 'NONE',  ( 3.000000000000000888, 18.80635025205187816, -13.23915371906935867 ) ) ;
#6496 = CARTESIAN_POINT ( 'NONE',  ( 0.000000000000000000, 0.000000000000000000, 0.000000000000000000 ) ) ;
#6497 = ORIENTED_EDGE ( 'NONE', *, *, #1800, .F. ) ;
#6498 = EDGE_LOOP ( 'NONE', ( #8099, #1737, #6644, #1843 ) ) ;
#6499 = EDGE_CURVE ( 'NONE', #10656, #10872, #1286, .T. ) ;
#6500 = CIRCLE ( 'NONE', #1838, 9.599999999999996092 ) ;
#6501 = FACE_OUTER_BOUND ( 'NONE', #8737, .T. ) ;
#6502 = VERTEX_POINT ( 'NONE', #12066 ) ;
#6503 = CIRCLE ( 'NONE', #1228, 24.80000000000000071 ) ;
#6504 = CARTESIAN_POINT ( 'NONE',  ( -3.432991321284826647, 4.402131891631369420, 3.747395293195558847E-16 ) ) ;
#6505 = CIRCLE ( 'NONE', #5926, 22.99899999999999878 ) ;
#6506 = FACE_BOUND ( 'NONE', #6950, .T. ) ;
#6507 = LINE ( 'NONE', #10242, #6985 ) ;
#6508 = DIRECTION ( 'NONE',  ( 0.000000000000000000, -0.2079116908177665313, 0.9781476007338041345 ) ) ;
#6509 = CARTESIAN_POINT ( 'NONE',  ( -11.80455809908110432, -11.41585333555581983, 10.00000000000000000 ) ) ;
#6510 = PRODUCT_RELATED_PRODUCT_CATEGORY ( 'part', '', ( #18 ) ) ;
#6511 = CIRCLE ( 'NONE', #8858, 24.80000000000000071 ) ;
#6512 = CARTESIAN_POINT ( 'NONE',  ( 6.396238541184324333, 6.183590428399971195, 6.857782953271941950E-17 ) ) ;
#6513 = EDGE_CURVE ( 'NONE', #1959, #9917, #8217, .T. ) ;
#6514 = CARTESIAN_POINT ( 'NONE',  ( 0.000000000000000000, 0.000000000000000000, 0.000000000000000000 ) ) ;
#6515 = CIRCLE ( 'NONE', #448, 24.80000000000000071 ) ;
#6516 = AXIS2_PLACEMENT_3D ( 'NONE', #537, #8930, #5995 ) ;
#6517 = ADVANCED_FACE ( 'NONE', ( #2775 ), #11945, .T. ) ;
#6518 = VERTEX_POINT ( 'NONE', #10110 ) ;
#6519 = ORIENTED_EDGE ( 'NONE', *, *, #6455, .T. ) ;
#6520 = AXIS2_PLACEMENT_3D ( 'NONE', #3795, #1946, #2008 ) ;
#6521 = DIRECTION ( 'NONE',  ( -1.000000000000000000, 0.000000000000000000, 0.000000000000000000 ) ) ;
#6522 = CARTESIAN_POINT ( 'NONE',  ( 10.00611923916671309, -2.842981073525690405, 10.00000000000000000 ) ) ;
#6523 = CYLINDRICAL_SURFACE ( 'NONE', #2489, 24.80000000000000071 ) ;
#6524 = DIRECTION ( 'NONE',  ( 1.000000000000000000, 0.000000000000000000, 0.000000000000000000 ) ) ;
#6525 = CARTESIAN_POINT ( 'NONE',  ( -1.307086582042907619, 11.26718560147321213, 3.747395293195558847E-16 ) ) ;
#6526 = CARTESIAN_POINT ( 'NONE',  ( 3.006682760306612856, 4.002877712838976976, 3.747395293195558847E-16 ) ) ;
#6527 = VECTOR ( 'NONE', #755, 1000.000000000000000 ) ;
#6528 = DIRECTION ( 'NONE',  ( 1.000000000000000000, 0.000000000000000000, -0.000000000000000000 ) ) ;
#6529 = VERTEX_POINT ( 'NONE', #1619 ) ;
#6530 = ORIENTED_EDGE ( 'NONE', *, *, #4874, .F. ) ;
#6531 = ORIENTED_EDGE ( 'NONE', *, *, #969, .F. ) ;
#6532 = LINE ( 'NONE', #5677, #5932 ) ;
#6533 = FACE_OUTER_BOUND ( 'NONE', #8584, .T. ) ;
#6534 = AXIS2_PLACEMENT_3D ( 'NONE', #1248, #376, #4115 ) ;
#6535 = CARTESIAN_POINT ( 'NONE',  ( 3.000000000000000888, 0.000000000000000000, 0.000000000000000000 ) ) ;
#6536 = CARTESIAN_POINT ( 'NONE',  ( 3.000000000000000888, -13.23915371906968019, 18.80635025205165078 ) ) ;
#6537 = ADVANCED_FACE ( 'NONE', ( #2529 ), #12011, .T. ) ;
#6538 = DIRECTION ( 'NONE',  ( -1.000000000000000000, 0.000000000000000000, -0.000000000000000000 ) ) ;
#6539 = CARTESIAN_POINT ( 'NONE',  ( 7.972781652389871354, 11.51689705412852405, 3.747395293195558847E-16 ) ) ;
#6540 = CARTESIAN_POINT ( 'NONE',  ( 1.737537816361722331, -4.672682311025833535, 6.857782953271941950E-17 ) ) ;
#6541 = DIRECTION ( 'NONE',  ( -1.000000000000000000, 0.000000000000000000, 0.000000000000000000 ) ) ;
#6542 = ORIENTED_EDGE ( 'NONE', *, *, #2048, .T. ) ;
#6543 = ORIENTED_EDGE ( 'NONE', *, *, #3689, .T. ) ;
#6544 = FACE_OUTER_BOUND ( 'NONE', #4419, .T. ) ;
#6545 = EDGE_CURVE ( 'NONE', #1864, #8369, #11636, .T. ) ;
#6546 = EDGE_LOOP ( 'NONE', ( #8575, #1834, #2194, #12048 ) ) ;
#6547 = ORIENTED_EDGE ( 'NONE', *, *, #5921, .T. ) ;
#6548 = DIRECTION ( 'NONE',  ( -1.000000000000000000, 0.000000000000000000, 0.000000000000000000 ) ) ;
#6549 = DIRECTION ( 'NONE',  ( -1.000000000000000000, 0.000000000000000000, -0.000000000000000000 ) ) ;
#6550 = VERTEX_POINT ( 'NONE', #7415 ) ;
#6551 = DIRECTION ( 'NONE',  ( -1.000000000000000000, 0.000000000000000000, 0.000000000000000000 ) ) ;
#6552 = CARTESIAN_POINT ( 'NONE',  ( 3.000000000000000888, 0.000000000000000000, 0.000000000000000000 ) ) ;
#6553 = CARTESIAN_POINT ( 'NONE',  ( -7.014275365397510065, 0.1192422097806477982, 10.00000000000000000 ) ) ;
#6554 = DIRECTION ( 'NONE',  ( 0.000000000000000000, 0.000000000000000000, 1.000000000000000000 ) ) ;
#6555 = DIRECTION ( 'NONE',  ( 0.000000000000000000, -0.8660254037844433705, 0.4999999999999919509 ) ) ;
#6556 = CARTESIAN_POINT ( 'NONE',  ( 3.000000000000000888, 20.65684170206491643, 13.72351598154904018 ) ) ;
#6557 = ORIENTED_EDGE ( 'NONE', *, *, #1451, .F. ) ;
#6558 = DIRECTION ( 'NONE',  ( -1.000000000000000000, 0.000000000000000000, -0.000000000000000000 ) ) ;
#6559 = ORIENTED_EDGE ( 'NONE', *, *, #938, .F. ) ;
#6560 = VECTOR ( 'NONE', #9993, 1000.000000000000000 ) ;
#6561 = CARTESIAN_POINT ( 'NONE',  ( 0.4634152073531427884, 14.27464310366533695, 10.00000000000000000 ) ) ;
#6562 = DIRECTION ( 'NONE',  ( 0.000000000000000000, 0.000000000000000000, -1.000000000000000000 ) ) ;
#6563 = SURFACE_STYLE_FILL_AREA ( #1117 ) ;
#6564 = CARTESIAN_POINT ( 'NONE',  ( 0.000000000000000000, -21.97702544527762214, 6.779701584702658046 ) ) ;
#6565 = LINE ( 'NONE', #4676, #5955 ) ;
#6566 = CARTESIAN_POINT ( 'NONE',  ( 0.2749788638910979355, -16.81181333738675931, 10.00000000000000000 ) ) ;
#6567 = AXIS2_PLACEMENT_3D ( 'NONE', #1174, #74, #7723 ) ;
#6568 = CARTESIAN_POINT ( 'NONE',  ( -7.014275365397503847, 0.1192422097806469378, 6.857782953271941950E-17 ) ) ;
#6569 = DIRECTION ( 'NONE',  ( -1.000000000000000000, 0.000000000000000000, -0.000000000000000000 ) ) ;
#6570 = DIRECTION ( 'NONE',  ( -1.000000000000000000, 0.000000000000000000, 0.000000000000000000 ) ) ;
#6571 = VERTEX_POINT ( 'NONE', #11161 ) ;
#6572 = ORIENTED_EDGE ( 'NONE', *, *, #11685, .F. ) ;
#6573 = ORIENTED_EDGE ( 'NONE', *, *, #9617, .T. ) ;
#6574 = CIRCLE ( 'NONE', #5017, 9.599999999999997868 ) ;
#6575 = CARTESIAN_POINT ( 'NONE',  ( 20.00000000000000000, 0.000000000000000000, -5.000000000000000000 ) ) ;
#6576 = CARTESIAN_POINT ( 'NONE',  ( -6.925491926712309620, 5.292860106065908177, 10.00000000000000000 ) ) ;
#6577 = EDGE_CURVE ( 'NONE', #11545, #4550, #6364, .T. ) ;
#6578 = CARTESIAN_POINT ( 'NONE',  ( 0.000000000000000000, 17.97274125076074114, 13.62355943574025652 ) ) ;
#6579 = EDGE_CURVE ( 'NONE', #9445, #5055, #12026, .T. ) ;
#6580 = EDGE_CURVE ( 'NONE', #1587, #2893, #5787, .T. ) ;
#6581 = CARTESIAN_POINT ( 'NONE',  ( 8.429646098664187903, -5.822225404888638600, 3.747395293195558847E-16 ) ) ;
#6582 = CARTESIAN_POINT ( 'NONE',  ( 0.000000000000000000, 20.65684170206509762, -13.72351598154876484 ) ) ;
#6583 = LINE ( 'NONE', #1816, #2563 ) ;
#6584 = VERTEX_POINT ( 'NONE', #3818 ) ;
#6585 = EDGE_LOOP ( 'NONE', ( #10583, #1227, #8204, #9257 ) ) ;
#6586 = ORIENTED_EDGE ( 'NONE', *, *, #9803, .T. ) ;
#6587 = EDGE_CURVE ( 'NONE', #117, #9866, #494, .T. ) ;
#6588 = DIRECTION ( 'NONE',  ( -1.000000000000000000, 0.000000000000000000, 0.000000000000000000 ) ) ;
#6589 = LINE ( 'NONE', #3720, #1392 ) ;
#6590 = CYLINDRICAL_SURFACE ( 'NONE', #7992, 9.599999999999997868 ) ;
#6591 = DIRECTION ( 'NONE',  ( -1.000000000000000000, 0.000000000000000000, 0.000000000000000000 ) ) ;
#6592 = VECTOR ( 'NONE', #1194, 1000.000000000000000 ) ;
#6593 = DIRECTION ( 'NONE',  ( 0.000000000000000000, 0.000000000000000000, 1.000000000000000000 ) ) ;
#6594 = CARTESIAN_POINT ( 'NONE',  ( -15.00596061316373842, -1.728743269517114323, 3.747395293195558847E-16 ) ) ;
#6595 = B_SPLINE_SURFACE_WITH_KNOTS ( 'NONE', 1, 3, ( 
 ( #6016, #10669, #9743, #4922, #5961, #9568, #9688, #1361, #5900, #5038, #1181, #6748, #1252, #11410, #4184, #10427, #8774, #4856, #4003, #11466, #5095, #3087, #4984, #1123, #9507, #8719, #8662, #4058, #5784, #7911, #7789, #5840, #379, #4120, #3031, #262, #7853, #10486, #11642, #2101, #6689, #1542, #6199, #11763, #560, #9924, #4294, #9810, #8095, #8028, #1483, #7040, #2340, #6077, #7101, #4239, #10851, #5278, #5218, #11822, #7157, #1424, #3388, #2460, #9012, #628, #3447, #4358, #3261, #6980, #10725, #2401, #10791, #5157, #8895, #500, #7965, #11698, #3320, #6143, #9871, #8951, #11299, #10312, #5737, #3713, #1930, #8431, #7433, #6525, #1746, #955, #10197, #11183, #8303, #5668, #5484, #2733, #31, #9220, #91, #9282, #10375, #2914, #6637, #897, #7499, #5553, #6581, #1996, #1875, #9399, #4632, #6462, #2797, #12027, #4812, #6401, #4756, #838, #12086, #10260, #9462, #5607, #4693, #4574, #3651, #9339, #8363, #3779, #7368, #1079, #11243, #1814, #1024, #3837, #7559, #10127, #2858, #8549, #8493, #146, #3891, #7611, #2670, #11112, #1617, #9135, #8216, #692, #12009, #3690, #1725, #813, #6385, #10238, #4554, #9260, #7348, #8284, #10174, #1790, #1855, #2651, #7226, #8346, #3457, #2597, #880, #5354, #7165, #10054, #5462, #9083, #11093, #7413, #5590, #2708, #5530, #8100, #4425, #4614, #12065, #8158, #3632, #9991, #936, #6504, #11159, #6442, #10976, #9190, #2774, #749, #9321, #11828, #11882, #10910, #3514, #2528, #4483, #6331, #6264, #5407, #1672, #11943, #3575, #7287 ),
 ( #11039, #10109, #9442, #8529, #3755, #2960, #73, #5715, #10296, #7660, #7477, #4738, #2035, #11222, #2094, #11282, #252, #4913, #8651, #2896, #9500, #7538, #8588, #3996, #3871, #185, #6619, #8475, #4793, #1913, #6797, #8406, #6740, #2838, #1973, #1062, #7722, #127, #6679, #6561, #5647, #7594, #10352, #11335, #9378, #11458, #10418, #3817, #3023, #5831, #9561, #5, #5775, #1173, #11401, #10477, #1114, #3078, #10533, #4847, #3935, #2151, #999, #5891, #9623, #4672, #8014, #11688, #9862, #8887, #11514, #7775, #5209, #4284, #6066, #8942, #6970, #9797, #11633, #3376, #1415, #2391, #491, #5149, #3306, #7090, #7902, #369, #1473, #8711, #7843, #6132, #10600, #312, #3200, #10714, #2214, #4229, #550, #10841, #7956, #10779, #1240, #5952, #11753, #2450, #6857, #7030, #3134, #6191, #4975, #4049, #9679, #4109, #2330, #1295, #2273, #5029, #8765, #11580, #6917, #10660, #6006, #9735, #1351, #5084, #8827, #430, #4175, #3250, #8143, #9120, #10037, #2637, #1600, #7394, #11994, #9175, #7331, #5265, #10092, #9916, #4538, #5336, #6371, #1531, #4349, #12052, #617, #11137, #731, #794, #3618, #2580, #677, #1711, #8083, #4599, #5391, #9977, #4466, #11811, #6427, #5445, #9001, #8267, #8202, #11928, #3558, #7270, #5514, #6314, #3439, #10156, #7149, #10898, #3673, #10959, #11079, #1773, #2512, #9069, #11024, #2692, #9245, #1659, #6249, #865, #8330, #2755, #4408, #11868, #3498, #7210, #10337, #10225, #1841, #10460, #12111, #7523, #6604, #11208, #10402, #5759, #3916, #5575, #6663, #6487 ) ),
 .UNSPECIFIED., .F., .F., .F.,
 ( 2, 2 ),
 ( 4, 2, 2, 2, 2, 2, 2, 2, 2, 2, 2, 2, 2, 2, 2, 2, 2, 2, 2, 2, 2, 2, 2, 2, 2, 2, 2, 2, 2, 2, 2, 2, 2, 2, 2, 2, 2, 2, 2, 2, 2, 2, 2, 2, 2, 2, 2, 2, 2, 2, 2, 2, 2, 2, 2, 2, 2, 2, 2, 2, 2, 2, 2, 2, 2, 2, 2, 2, 2, 2, 2, 2, 2, 2, 2, 2, 2, 2, 2, 2, 2, 2, 2, 2, 2, 2, 2, 2, 2, 2, 2, 2, 2, 2, 2, 2, 2, 2, 2, 2, 2, 2, 2, 4 ),
 ( 0.4999999999999998890, 0.9545454545454546968 ),
 ( 0.000000000000000000, 0.007812500000000000000, 0.01562500000000000000, 0.02343750000000000000, 0.03125000000000000000, 0.03906250000000000000, 0.04687500000000000000, 0.05468750000000000000, 0.06250000000000000000, 0.07031250000000000000, 0.07812500000000000000, 0.08593750000000000000, 0.09375000000000000000, 0.1015625000000000000, 0.1093750000000000000, 0.1171875000000000000, 0.1250000000000000000, 0.1328125000000000000, 0.1406250000000000000, 0.1484375000000000000, 0.1562500000000000000, 0.1640625000000000000, 0.1718750000000000000, 0.1796875000000000000, 0.1875000000000000000, 0.1953125000000000000, 0.2031250000000000000, 0.2109375000000000000, 0.2187500000000000000, 0.2265625000000000000, 0.2343750000000000000, 0.2421875000000000000, 0.2500000000000000000, 0.2578125000000000000, 0.2656250000000000000, 0.2734375000000000000, 0.2812500000000000000, 0.2890625000000000000, 0.2968750000000000000, 0.3046875000000000000, 0.3125000000000000000, 0.3203125000000000000, 0.3281250000000000000, 0.3359375000000000000, 0.3437500000000000000, 0.3515625000000000000, 0.3593750000000000000, 0.3671875000000000000, 0.3750000000000000000, 0.3828125000000000000, 0.3906250000000000000, 0.3984375000000000000, 0.4062500000000000000, 0.4140625000000000000, 0.4218750000000000000, 0.4296875000000000000, 0.4375000000000000000, 0.4453125000000000000, 0.4531250000000000000, 0.4609375000000000000, 0.4687500000000000000, 0.4765625000000000000, 0.4843750000000000000, 0.4921875000000000000, 0.5000000000000000000, 0.5078125000000000000, 0.5156250000000000000, 0.5234375000000000000, 0.5312500000000000000, 0.5390625000000000000, 0.5468750000000000000, 0.5546875000000000000, 0.5625000000000000000, 0.5703125000000000000, 0.5781250000000000000, 0.5859375000000000000, 0.5937500000000000000, 0.6015625000000000000, 0.6093750000000000000, 0.6171875000000000000, 0.6250000000000000000, 0.6328125000000000000, 0.6406250000000000000, 0.6484375000000000000, 0.6562500000000000000, 0.6640625000000000000, 0.6718750000000000000, 0.6796875000000000000, 0.6875000000000000000, 0.6953125000000000000, 0.7031250000000000000, 0.7109375000000000000, 0.7187500000000000000, 0.7265625000000000000, 0.7343750000000000000, 0.7421875000000000000, 0.7500000000000000000, 0.7656250000000000000, 0.7812500000000000000, 0.7968750000000000000, 0.8125000000000000000, 0.8281250000000000000, 0.8437500000000000000, 0.8499999999999999778 ),
 .UNSPECIFIED. ) ;
#6596 = ADVANCED_FACE ( 'NONE', ( #255 ), #10479, .T. ) ;
#6597 = CARTESIAN_POINT ( 'NONE',  ( 3.000000000000000888, 0.000000000000000000, 0.000000000000000000 ) ) ;
#6598 = ORIENTED_EDGE ( 'NONE', *, *, #11596, .T. ) ;
#6599 = ORIENTED_EDGE ( 'NONE', *, *, #2844, .T. ) ;
#6600 = LINE ( 'NONE', #4831, #5308 ) ;
#6601 = ORIENTED_EDGE ( 'NONE', *, *, #11661, .T. ) ;
#6602 = EDGE_CURVE ( 'NONE', #6896, #662, #2453, .T. ) ;
#6603 = AXIS2_PLACEMENT_3D ( 'NONE', #10098, #11084, #3565 ) ;
#6604 = CARTESIAN_POINT ( 'NONE',  ( 4.340769014460005515, -0.9713985772308084687, 10.00000000000000000 ) ) ;
#6605 = CYLINDRICAL_SURFACE ( 'NONE', #4430, 3.000000000000000444 ) ;
#6606 = EDGE_LOOP ( 'NONE', ( #1545, #1976, #7734, #4230 ) ) ;
#6607 = CYLINDRICAL_SURFACE ( 'NONE', #7485, 24.80000000000000071 ) ;
#6608 = EDGE_CURVE ( 'NONE', #9071, #6916, #8408, .T. ) ;
#6609 = LINE ( 'NONE', #2885, #230 ) ;
#6610 = CARTESIAN_POINT ( 'NONE',  ( 1.748316258820581170, 15.14524454193558611, 6.857782953271941950E-17 ) ) ;
#6611 = CIRCLE ( 'NONE', #4078, 9.599999999999997868 ) ;
#6612 = DIRECTION ( 'NONE',  ( -1.000000000000000000, 0.000000000000000000, -0.000000000000000000 ) ) ;
#6613 = CARTESIAN_POINT ( 'NONE',  ( 3.000000000000000888, 11.48910920600683738, 21.97817939804043519 ) ) ;
#6614 = EDGE_LOOP ( 'NONE', ( #2433, #10050, #7634, #520 ) ) ;
#6615 = EDGE_LOOP ( 'NONE', ( #6667, #2633, #12107, #109 ) ) ;
#6616 = CARTESIAN_POINT ( 'NONE',  ( 3.000000000000000888, 15.42759117534385993, 16.45023496161670451 ) ) ;
#6617 = ORIENTED_EDGE ( 'NONE', *, *, #2025, .F. ) ;
#6618 = EDGE_CURVE ( 'NONE', #11471, #11794, #8729, .T. ) ;
#6619 = CARTESIAN_POINT ( 'NONE',  ( -15.05755265055531389, -0.4891349978715465729, 10.00000000000000000 ) ) ;
#6620 = AXIS2_PLACEMENT_3D ( 'NONE', #6050, #6780, #9777 ) ;
#6621 = DIRECTION ( 'NONE',  ( 0.000000000000000000, 0.000000000000000000, 1.000000000000000000 ) ) ;
#6622 = PRESENTATION_STYLE_ASSIGNMENT (( #4849 ) ) ;
#6623 = CARTESIAN_POINT ( 'NONE',  ( 1.500000000000000444, 13.72351598154897268, 20.65684170206496262 ) ) ;
#6624 = EDGE_CURVE ( 'NONE', #4337, #2865, #10671, .T. ) ;
#6625 = CYLINDRICAL_SURFACE ( 'NONE', #1066, 9.599999999999997868 ) ;
#6626 = CARTESIAN_POINT ( 'NONE',  ( 0.000000000000000000, 6.532525787311267429, -21.58580335785669746 ) ) ;
#6627 = CARTESIAN_POINT ( 'NONE',  ( 3.000000000000000888, -23.88662356770110762, -6.668524164681871369 ) ) ;
#6628 = DIRECTION ( 'NONE',  ( -1.000000000000000000, 0.000000000000000000, 0.000000000000000000 ) ) ;
#6629 = CARTESIAN_POINT ( 'NONE',  ( 3.000000000000000888, 0.000000000000000000, 0.000000000000000000 ) ) ;
#6630 = ORIENTED_EDGE ( 'NONE', *, *, #5721, .T. ) ;
#6631 = CARTESIAN_POINT ( 'NONE',  ( -4.500000000000000000, 0.4999999999999998890, 3.000000000000000000 ) ) ;
#6632 = ORIENTED_EDGE ( 'NONE', *, *, #2854, .F. ) ;
#6633 = CYLINDRICAL_SURFACE ( 'NONE', #3631, 22.99899999999999878 ) ;
#6634 = CARTESIAN_POINT ( 'NONE',  ( 3.053028024665676021, -9.450988318042126579, 10.00000000000000000 ) ) ;
#6635 = DIRECTION ( 'NONE',  ( 0.000000000000000000, 0.4067366430758009299, -0.9135454576426005335 ) ) ;
#6636 = AXIS2_PLACEMENT_3D ( 'NONE', #5063, #4208, #1327 ) ;
#6637 = CARTESIAN_POINT ( 'NONE',  ( 10.41236255589546822, -1.188820951657898473, 3.747395293195558847E-16 ) ) ;
#6638 = CARTESIAN_POINT ( 'NONE',  ( 0.000000000000000000, 4.898587196589412829E-16, -4.000000000000000000 ) ) ;
#6639 = ORIENTED_EDGE ( 'NONE', *, *, #5866, .F. ) ;
#6640 = VECTOR ( 'NONE', #5051, 1000.000000000000000 ) ;
#6641 = ORIENTED_EDGE ( 'NONE', *, *, #90, .F. ) ;
#6642 = EDGE_CURVE ( 'NONE', #3296, #3787, #9698, .T. ) ;
#6643 = AXIS2_PLACEMENT_3D ( 'NONE', #6693, #383, #8842 ) ;
#6644 = ORIENTED_EDGE ( 'NONE', *, *, #833, .T. ) ;
#6645 = CARTESIAN_POINT ( 'NONE',  ( 0.000000000000000000, 0.000000000000000000, -15.00000000000000000 ) ) ;
#6646 = DIRECTION ( 'NONE',  ( 0.000000000000000000, 0.000000000000000000, 1.000000000000000000 ) ) ;
#6647 = ORIENTED_EDGE ( 'NONE', *, *, #11197, .F. ) ;
#6648 = LINE ( 'NONE', #9412, #1353 ) ;
#6649 = DIRECTION ( 'NONE',  ( 1.000000000000000000, -0.000000000000000000, 0.000000000000000000 ) ) ;
#6650 = CIRCLE ( 'NONE', #4117, 9.599999999999997868 ) ;
#6651 = CYLINDRICAL_SURFACE ( 'NONE', #11023, 22.99899999999999878 ) ;
#6652 = VECTOR ( 'NONE', #1766, 1000.000000000000000 ) ;
#6653 = AXIS2_PLACEMENT_3D ( 'NONE', #10657, #5949, #8526 ) ;
#6654 = CARTESIAN_POINT ( 'NONE',  ( -1.036640877615904843, -15.73686152240404468, 3.747395293195558847E-16 ) ) ;
#6655 = EDGE_CURVE ( 'NONE', #4944, #7927, #7479, .T. ) ;
#6656 = ADVANCED_FACE ( 'NONE', ( #2839 ), #8590, .T. ) ;
#6657 = FACE_OUTER_BOUND ( 'NONE', #1580, .T. ) ;
#6658 = VERTEX_POINT ( 'NONE', #11402 ) ;
#6659 = ORIENTED_EDGE ( 'NONE', *, *, #11707, .F. ) ;
#6660 = DIRECTION ( 'NONE',  ( 1.000000000000000000, 0.000000000000000000, 0.000000000000000000 ) ) ;
#6661 = AXIS2_PLACEMENT_3D ( 'NONE', #7041, #6145, #8469 ) ;
#6662 = VERTEX_POINT ( 'NONE', #7596 ) ;
#6663 = CARTESIAN_POINT ( 'NONE',  ( 0.3190826481552657135, -3.778307095988849618, 10.00000000000000000 ) ) ;
#6664 = AXIS2_PLACEMENT_3D ( 'NONE', #4463, #9302, #9173 ) ;
#6665 = VECTOR ( 'NONE', #9409, 1000.000000000000000 ) ;
#6666 = LINE ( 'NONE', #6726, #2666 ) ;
#6667 = ORIENTED_EDGE ( 'NONE', *, *, #6898, .F. ) ;
#6668 = CARTESIAN_POINT ( 'NONE',  ( 0.000000000000000000, 0.000000000000000000, 4.000000000000000000 ) ) ;
#6669 = CYLINDRICAL_SURFACE ( 'NONE', #4745, 24.80000000000000071 ) ;
#6670 = CARTESIAN_POINT ( 'NONE',  ( -7.159234172427924925, 10.34564589702410942, 6.857782953271941950E-17 ) ) ;
#6671 = AXIS2_PLACEMENT_3D ( 'NONE', #10802, #4135, #332 ) ;
#6672 = PRODUCT_DEFINITION_SHAPE ( 'NONE', 'NONE',  #12122 ) ;
#6673 = DIRECTION ( 'NONE',  ( 1.000000000000000000, -0.000000000000000000, -0.000000000000000000 ) ) ;
#6674 = CARTESIAN_POINT ( 'NONE',  ( 3.000000000000000888, -21.97702544527762214, 6.779701584702658046 ) ) ;
#6675 = VERTEX_POINT ( 'NONE', #1857 ) ;
#6676 = EDGE_LOOP ( 'NONE', ( #9493, #6086, #7820, #7389 ) ) ;
#6677 = FACE_OUTER_BOUND ( 'NONE', #3841, .T. ) ;
#6678 = ORIENTED_EDGE ( 'NONE', *, *, #7618, .F. ) ;
#6679 = CARTESIAN_POINT ( 'NONE',  ( -1.872083171988683015, 14.23747171912756393, 10.00000000000000000 ) ) ;
#6680 = AXIS2_PLACEMENT_3D ( 'NONE', #11641, #10850, #9923 ) ;
#6681 = VECTOR ( 'NONE', #9856, 1000.000000000000000 ) ;
#6682 = DIRECTION ( 'NONE',  ( -1.000000000000000000, -0.000000000000000000, -0.000000000000000000 ) ) ;
#6683 = ORIENTED_EDGE ( 'NONE', *, *, #4649, .F. ) ;
#6684 = CARTESIAN_POINT ( 'NONE',  ( -10.00000000000000000, 0.000000000000000000, 0.000000000000000000 ) ) ;
#6685 = DIRECTION ( 'NONE',  ( -1.000000000000000000, 0.000000000000000000, 0.000000000000000000 ) ) ;
#6686 = CARTESIAN_POINT ( 'NONE',  ( -9.783806739528735363, -9.162509837619124298, 10.00000000000000000 ) ) ;
#6687 = EDGE_CURVE ( 'NONE', #4410, #264, #6759, .T. ) ;
#6688 = SURFACE_STYLE_FILL_AREA ( #6747 ) ;
#6689 = CARTESIAN_POINT ( 'NONE',  ( 1.629745903656676376, 14.14889381255349932, 3.747395293195558847E-16 ) ) ;
#6690 = FACE_OUTER_BOUND ( 'NONE', #6119, .T. ) ;
#6691 = AXIS2_PLACEMENT_3D ( 'NONE', #2569, #3491, #7201 ) ;
#6692 = ORIENTED_EDGE ( 'NONE', *, *, #609, .F. ) ;
#6693 = CARTESIAN_POINT ( 'NONE',  ( 3.000000000000000888, 6.532525787310969001, 21.58580335785678983 ) ) ;
#6694 = ADVANCED_FACE ( 'NONE', ( #2961 ), #3997, .T. ) ;
#6695 = EDGE_LOOP ( 'NONE', ( #6062, #2455, #2694, #9148 ) ) ;
#6696 = DIRECTION ( 'NONE',  ( 0.000000000000000000, -0.4067366430758071472, 0.9135454576425979800 ) ) ;
#6697 = CARTESIAN_POINT ( 'NONE',  ( 6.723006375386864519, 3.907299473125435796, 10.00000000000000000 ) ) ;
#6698 = SHAPE_REPRESENTATION ( 'arbor', ( #8474 ), #1578 ) ;
#6699 = CIRCLE ( 'NONE', #6327, 4.000000000000000000 ) ;
#6700 = CARTESIAN_POINT ( 'NONE',  ( 3.000000000000000888, 7.432877647175492264, -21.76479567747234256 ) ) ;
#6701 = CARTESIAN_POINT ( 'NONE',  ( 7.252227276002106038, 5.017415995114419047, 10.00000000000000000 ) ) ;
#6702 = AXIS2_PLACEMENT_3D ( 'NONE', #9048, #8250, #6115 ) ;
#6703 = AXIS2_PLACEMENT_3D ( 'NONE', #1799, #5538, #4800 ) ;
#6704 = CARTESIAN_POINT ( 'NONE',  ( -10.85385039129052842, -12.37615246896657339, 6.857782953271941950E-17 ) ) ;
#6705 = CARTESIAN_POINT ( 'NONE',  ( 0.000000000000000000, 22.15038895030649257, 4.240409074144170454 ) ) ;
#6706 = EDGE_LOOP ( 'NONE', ( #9033, #1276, #3628, #5340, #7347, #3510, #4535, #8080, #9117, #2065, #10447, #2354, #4423, #1410, #7692, #4514, #11719, #3115, #10014, #8013, #7718, #1457, #1697, #2513, #1687, #7060, #593, #11338, #6543, #11091, #37, #11263, #4715, #7782, #5701, #3355, #7016, #6053, #4452, #2686, #4806, #4276, #7269, #2923, #3676, #10548, #6421, #10003, #11058, #4859, #2674, #6279, #8181, #8996, #1714, #7392, #10237, #3993, #11510, #10379, #9259, #9456, #11060, #6519, #2689, #5166, #920, #2938, #1129, #9147, #11681, #9376, #594, #2724, #7069, #4565, #10034, #10284, #124, #9157, #6531, #5627, #11104, #2017, #8587, #5256, #10413, #1807, #6707, #6586, #2540, #2758, #10577, #1162, #5824, #3735, #792, #1840, #211, #9876, #7689, #6133, #1923, #11946, #9510, #16, #3322, #3800, #4127, #3731, #1155, #2861, #184, #1104, #3601, #2241, #5931, #3065, #10432, #11163, #10854, #8501, #3198, #2202, #2296, #54, #9799, #7901, #7046, #6129, #4093, #10219, #1206, #2805, #5018, #8676, #4816, #10474, #2165, #10549, #9932, #503, #7032, #4213, #5224, #6871, #3950, #229, #6721, #9815, #9514, #11483, #8631, #1275, #10104, #6897, #5025, #5377, #7008, #797, #5964, #9649, #11691, #9616, #10784, #1058, #5711, #688, #1968, #4669, #1786, #3343, #11628, #10884, #3015, #2074, #4500, #1219, #2789, #337, #932, #3177, #5054, #8828, #6020, #11730, #1089, #10078, #548, #11717, #1316, #12062, #11871, #6440, #812, #10118, #5512, #10018, #7208, #7131, #4233, #5528, #9122, #4052, #7241, #4031, #8132, #5349, #2556, #5299, #10090, #10811, #11785, #4997, #12053, #1237, #8124, #8985, #6171, #6791, #3525, #3438, #11303, #3740, #4407, #2000, #1126, #3802, #10415, #8215, #8168, #2910, #6598, #8567, #5629, #8003, #1130, #5557, #2579, #5488, #1969, #7574, #2609, #5559, #8453 ) ) ;
#6707 = ORIENTED_EDGE ( 'NONE', *, *, #8864, .F. ) ;
#6708 = CIRCLE ( 'NONE', #7688, 9.599999999999997868 ) ;
#6709 = ORIENTED_EDGE ( 'NONE', *, *, #3739, .F. ) ;
#6710 = DIRECTION ( 'NONE',  ( -1.000000000000000000, -0.000000000000000000, -0.000000000000000000 ) ) ;
#6711 = DIRECTION ( 'NONE',  ( 0.000000000000000000, 0.000000000000000000, -1.000000000000000000 ) ) ;
#6712 = ORIENTED_EDGE ( 'NONE', *, *, #5368, .F. ) ;
#6713 = DIRECTION ( 'NONE',  ( 0.000000000000000000, 0.2079116908177532086, 0.9781476007338069101 ) ) ;
#6714 = CARTESIAN_POINT ( 'NONE',  ( 3.000000000000000888, -11.79560690673886292, 19.74380051311536022 ) ) ;
#6715 = LINE ( 'NONE', #10864, #9075 ) ;
#6716 = CARTESIAN_POINT ( 'NONE',  ( 11.72652038055309731, 7.297668919379284524, 3.747395293195558847E-16 ) ) ;
#6717 = DIRECTION ( 'NONE',  ( -1.000000000000000000, -0.000000000000000000, -0.000000000000000000 ) ) ;
#6718 = ORIENTED_EDGE ( 'NONE', *, *, #12105, .F. ) ;
#6719 = VERTEX_POINT ( 'NONE', #7663 ) ;
#6720 = DIRECTION ( 'NONE',  ( 0.000000000000000000, 0.000000000000000000, -1.000000000000000000 ) ) ;
#6721 = ORIENTED_EDGE ( 'NONE', *, *, #6587, .F. ) ;
#6722 = CIRCLE ( 'NONE', #1449, 9.599999999999997868 ) ;
#6723 = DIRECTION ( 'NONE',  ( -1.000000000000000000, -0.000000000000000000, 0.000000000000000000 ) ) ;
#6724 = CARTESIAN_POINT ( 'NONE',  ( 0.000000000000000000, 0.000000000000000000, 0.000000000000000000 ) ) ;
#6725 = ADVANCED_FACE ( 'NONE', ( #1000 ), #8478, .T. ) ;
#6726 = CARTESIAN_POINT ( 'NONE',  ( 1.499999999999999556, -9.128825345752876075, -23.05871956130131650 ) ) ;
#6727 = EDGE_LOOP ( 'NONE', ( #10412, #3424, #2494, #11668 ) ) ;
#6728 = EDGE_CURVE ( 'NONE', #5072, #10349, #6374, .T. ) ;
#6729 = CARTESIAN_POINT ( 'NONE',  ( 3.000000000000000888, -22.47229024614976112, -1.901833551798492561 ) ) ;
#6730 = ADVANCED_FACE ( 'NONE', ( #5650, #6506 ), #5591, .T. ) ;
#6731 = DIRECTION ( 'NONE',  ( 1.000000000000000000, -0.000000000000000000, -0.000000000000000000 ) ) ;
#6732 = CARTESIAN_POINT ( 'NONE',  ( 5.564773995946417529, -12.83798980516507626, 6.857782953271941950E-17 ) ) ;
#6733 = CIRCLE ( 'NONE', #8304, 24.80000000000000071 ) ;
#6734 = DIRECTION ( 'NONE',  ( 0.000000000000000000, -0.3090169943749544457, 0.9510565162951514218 ) ) ;
#6735 = VERTEX_POINT ( 'NONE', #11689 ) ;
#6736 = CARTESIAN_POINT ( 'NONE',  ( 3.000000000000000888, 0.000000000000000000, 0.000000000000000000 ) ) ;
#6737 = ORIENTED_EDGE ( 'NONE', *, *, #3544, .T. ) ;
#6738 = DIRECTION ( 'NONE',  ( -1.000000000000000000, 0.000000000000000000, -0.000000000000000000 ) ) ;
#6739 = ORIENTED_EDGE ( 'NONE', *, *, #11298, .F. ) ;
#6740 = CARTESIAN_POINT ( 'NONE',  ( -11.21689850596896676, 9.520844388990630236, 10.00000000000000000 ) ) ;
#6741 = EDGE_CURVE ( 'NONE', #1245, #10167, #4976, .T. ) ;
#6742 = DIRECTION ( 'NONE',  ( 0.000000000000000000, 0.000000000000000000, 1.000000000000000000 ) ) ;
#6743 = ORIENTED_EDGE ( 'NONE', *, *, #4582, .F. ) ;
#6744 = DIRECTION ( 'NONE',  ( -1.000000000000000000, -0.000000000000000000, -0.000000000000000000 ) ) ;
#6745 = DIRECTION ( 'NONE',  ( -1.000000000000000000, 0.000000000000000000, 0.000000000000000000 ) ) ;
#6746 = CARTESIAN_POINT ( 'NONE',  ( 6.986659217179110648, 9.748146710219847577, 10.00000000000000000 ) ) ;
#6747 = FILL_AREA_STYLE ('',( #8661 ) ) ;
#6748 = CARTESIAN_POINT ( 'NONE',  ( 4.123629756449401107, -15.38522696314584515, 3.747395293195558847E-16 ) ) ;
#6749 = DIRECTION ( 'NONE',  ( -1.000000000000000000, 0.000000000000000000, 0.000000000000000000 ) ) ;
#6750 = EDGE_CURVE ( 'NONE', #7795, #8063, #11457, .T. ) ;
#6751 = ORIENTED_EDGE ( 'NONE', *, *, #8843, .T. ) ;
#6752 = AXIS2_PLACEMENT_3D ( 'NONE', #9501, #9322, #6562 ) ;
#6753 = FACE_OUTER_BOUND ( 'NONE', #6370, .T. ) ;
#6754 = ORIENTED_EDGE ( 'NONE', *, *, #10598, .F. ) ;
#6755 = EDGE_CURVE ( 'NONE', #11218, #1648, #4287, .T. ) ;
#6756 = DIRECTION ( 'NONE',  ( 0.000000000000000000, 0.000000000000000000, 1.000000000000000000 ) ) ;
#6757 = CARTESIAN_POINT ( 'NONE',  ( -5.962113107391272315, -1.426310550302921865, 10.00000000000000000 ) ) ;
#6758 = DIRECTION ( 'NONE',  ( -1.000000000000000000, -0.000000000000000000, -0.000000000000000000 ) ) ;
#6759 = CIRCLE ( 'NONE', #4025, 9.599999999999997868 ) ;
#6760 = CARTESIAN_POINT ( 'NONE',  ( 8.527474615971327054, 0.9793716136081388468, 10.00000000000000000 ) ) ;
#6761 = CARTESIAN_POINT ( 'NONE',  ( -9.080917052262540423, 12.68274194616037320, 6.857782953271941950E-17 ) ) ;
#6762 = EDGE_CURVE ( 'NONE', #6502, #1587, #5211, .T. ) ;
#6763 = APPLICATION_CONTEXT ( 'automotive_design' ) ;
#6764 = DIRECTION ( 'NONE',  ( 0.000000000000000000, 0.000000000000000000, 1.000000000000000000 ) ) ;
#6765 = ORIENTED_EDGE ( 'NONE', *, *, #214, .F. ) ;
#6766 = VECTOR ( 'NONE', #5434, 1000.000000000000000 ) ;
#6767 = ORIENTED_EDGE ( 'NONE', *, *, #7699, .F. ) ;
#6768 = CARTESIAN_POINT ( 'NONE',  ( -10.00000000000000000, 0.000000000000000000, 0.000000000000000000 ) ) ;
#6769 = CARTESIAN_POINT ( 'NONE',  ( 13.68367311611256909, -8.822018488634764566, 10.00000000000000000 ) ) ;
#6770 = CARTESIAN_POINT ( 'NONE',  ( 1.500000000000000444, 15.40502424595145214, 19.43515443678408161 ) ) ;
#6771 = DIRECTION ( 'NONE',  ( -1.000000000000000000, -0.000000000000000000, 0.000000000000000000 ) ) ;
#6772 = CARTESIAN_POINT ( 'NONE',  ( 8.800885721068835821, 6.316044917328127895, 3.747395293195558847E-16 ) ) ;
#6773 = CARTESIAN_POINT ( 'NONE',  ( 3.000000000000000888, 0.000000000000000000, 0.000000000000000000 ) ) ;
#6774 = ORIENTED_EDGE ( 'NONE', *, *, #5714, .T. ) ;
#6775 = ORIENTED_EDGE ( 'NONE', *, *, #4862, .F. ) ;
#6776 = APPLICATION_PROTOCOL_DEFINITION ( 'draft international standard', 'automotive_design', 1998, #3874 ) ;
#6777 = CARTESIAN_POINT ( 'NONE',  ( -5.101271054653082615, -15.85638610327791476, 10.00000000000000000 ) ) ;
#6778 = ORIENTED_EDGE ( 'NONE', *, *, #11223, .T. ) ;
#6779 = CARTESIAN_POINT ( 'NONE',  ( 4.382127860174850120, -16.35473703246190524, 6.857782953271941950E-17 ) ) ;
#6780 = DIRECTION ( 'NONE',  ( -1.000000000000000000, -0.000000000000000000, 0.000000000000000000 ) ) ;
#6781 = LINE ( 'NONE', #418, #8870 ) ;
#6782 = FACE_OUTER_BOUND ( 'NONE', #7994, .T. ) ;
#6783 = ORIENTED_EDGE ( 'NONE', *, *, #5241, .F. ) ;
#6784 = LINE ( 'NONE', #10464, #2010 ) ;
#6785 = CARTESIAN_POINT ( 'NONE',  ( 0.000000000000000000, 0.000000000000000000, 0.000000000000000000 ) ) ;
#6786 = CARTESIAN_POINT ( 'NONE',  ( -6.864300873105353418, 13.92024697337931549, 6.857782953271941950E-17 ) ) ;
#6787 = DIRECTION ( 'NONE',  ( -1.000000000000000000, 0.000000000000000000, 0.000000000000000000 ) ) ;
#6788 = VERTEX_POINT ( 'NONE', #7844 ) ;
#6789 = FACE_OUTER_BOUND ( 'NONE', #4037, .T. ) ;
#6790 = VECTOR ( 'NONE', #10042, 1000.000000000000000 ) ;
#6791 = ORIENTED_EDGE ( 'NONE', *, *, #10097, .T. ) ;
#6792 = CARTESIAN_POINT ( 'NONE',  ( 3.000000000000000888, 0.000000000000000000, 0.000000000000000000 ) ) ;
#6793 = ADVANCED_FACE ( 'NONE', ( #552 ), #2394, .T. ) ;
#6794 = ORIENTED_EDGE ( 'NONE', *, *, #11961, .F. ) ;
#6795 = EDGE_CURVE ( 'NONE', #7721, #8331, #9498, .T. ) ;
#6796 = EDGE_CURVE ( 'NONE', #3911, #6334, #1294, .T. ) ;
#6797 = CARTESIAN_POINT ( 'NONE',  ( -13.29946171776686903, 6.562258890817373569, 10.00000000000000000 ) ) ;
#6798 = DIRECTION ( 'NONE',  ( 1.000000000000000000, 0.000000000000000000, 0.000000000000000000 ) ) ;
#6799 = AXIS2_PLACEMENT_3D ( 'NONE', #11487, #6771, #6893 ) ;
#6800 = DIRECTION ( 'NONE',  ( -1.000000000000000000, -0.000000000000000000, 0.000000000000000000 ) ) ;
#6801 = AXIS2_PLACEMENT_3D ( 'NONE', #6944, #7876, #5121 ) ;
#6802 = CARTESIAN_POINT ( 'NONE',  ( 0.000000000000000000, 0.000000000000000000, 0.000000000000000000 ) ) ;
#6803 = CARTESIAN_POINT ( 'NONE',  ( 4.165359127293308816, 14.58480927028733554, 10.00000000000000000 ) ) ;
#6804 = DIRECTION ( 'NONE',  ( -1.000000000000000000, 0.000000000000000000, -0.000000000000000000 ) ) ;
#6805 = EDGE_CURVE ( 'NONE', #11900, #11379, #1354, .T. ) ;
#6806 = FACE_OUTER_BOUND ( 'NONE', #2181, .T. ) ;
#6807 = CARTESIAN_POINT ( 'NONE',  ( 3.000000000000000888, 24.02068490260612776, 6.168200451485839508 ) ) ;
#6808 = ADVANCED_FACE ( 'NONE', ( #1243 ), #4051, .F. ) ;
#6809 = CIRCLE ( 'NONE', #8161, 9.599999999999997868 ) ;
#6810 = ORIENTED_EDGE ( 'NONE', *, *, #4034, .T. ) ;
#6811 = ORIENTED_EDGE ( 'NONE', *, *, #6357, .T. ) ;
#6812 = CARTESIAN_POINT ( 'NONE',  ( 0.000000000000000000, 0.000000000000000000, 3.000000000000000000 ) ) ;
#6813 = CARTESIAN_POINT ( 'NONE',  ( 7.527773320476329744, 0.8933511214756656438, 10.00000000000000000 ) ) ;
#6814 = DIRECTION ( 'NONE',  ( 0.000000000000000000, 0.000000000000000000, 1.000000000000000000 ) ) ;
#6815 = CARTESIAN_POINT ( 'NONE',  ( 0.7062845326068618590, -10.79445016380499212, 10.00000000000000000 ) ) ;
#6816 = AXIS2_PLACEMENT_3D ( 'NONE', #3361, #9214, #10828 ) ;
#6817 = CARTESIAN_POINT ( 'NONE',  ( 4.165359127293307040, 14.58480927028732843, 6.857782953271941950E-17 ) ) ;
#6818 = FACE_OUTER_BOUND ( 'NONE', #7792, .T. ) ;
#6819 = DIRECTION ( 'NONE',  ( 0.000000000000000000, 0.5877852522924741363, -0.8090169943749467851 ) ) ;
#6820 = ORIENTED_EDGE ( 'NONE', *, *, #2025, .T. ) ;
#6821 = ORIENTED_EDGE ( 'NONE', *, *, #3830, .F. ) ;
#6822 = DIRECTION ( 'NONE',  ( -1.000000000000000000, 0.000000000000000000, 0.000000000000000000 ) ) ;
#6823 = AXIS2_PLACEMENT_3D ( 'NONE', #10505, #8445, #4767 ) ;
#6824 = CARTESIAN_POINT ( 'NONE',  ( 12.88139461472802516, -9.891864711285373701, 10.00000000000000000 ) ) ;
#6825 = AXIS2_PLACEMENT_3D ( 'NONE', #4088, #1510, #592 ) ;
#6826 = DIRECTION ( 'NONE',  ( 0.000000000000000000, 0.000000000000000000, 1.000000000000000000 ) ) ;
#6827 = DIRECTION ( 'NONE',  ( 0.000000000000000000, 0.000000000000000000, 1.000000000000000000 ) ) ;
#6828 = CARTESIAN_POINT ( 'NONE',  ( 4.583115687978880359, -8.898851689028539624, 3.747395293195558847E-16 ) ) ;
#6829 = AXIS2_PLACEMENT_3D ( 'NONE', #1264, #8734, #8911 ) ;
#6830 = EDGE_CURVE ( 'NONE', #5828, #5674, #107, .T. ) ;
#6831 = AXIS2_PLACEMENT_3D ( 'NONE', #5313, #3480, #4748 ) ;
#6832 = DIRECTION ( 'NONE',  ( -1.000000000000000000, 0.000000000000000000, -0.000000000000000000 ) ) ;
#6833 = EDGE_LOOP ( 'NONE', ( #4421, #5351, #6951, #278 ) ) ;
#6834 = VERTEX_POINT ( 'NONE', #7957 ) ;
#6835 = APPLICATION_PROTOCOL_DEFINITION ( 'draft international standard', 'automotive_design', 1998, #1138 ) ;
#6836 = CARTESIAN_POINT ( 'NONE',  ( -9.080917052262543976, 12.68274194616037853, 10.00000000000000000 ) ) ;
#6837 = VERTEX_POINT ( 'NONE', #6858 ) ;
#6838 = DIRECTION ( 'NONE',  ( -1.000000000000000000, -0.000000000000000000, -0.000000000000000000 ) ) ;
#6839 = CARTESIAN_POINT ( 'NONE',  ( 3.000000000000000888, 10.87771529938188486, -19.75591328264875202 ) ) ;
#6840 = ADVANCED_FACE ( 'NONE', ( #2217 ), #7904, .T. ) ;
#6841 = AXIS2_PLACEMENT_3D ( 'NONE', #10363, #2784, #9207 ) ;
#6842 = DIRECTION ( 'NONE',  ( 0.000000000000000000, 0.000000000000000000, 1.000000000000000000 ) ) ;
#6843 = AXIS2_PLACEMENT_3D ( 'NONE', #8939, #610, #11806 ) ;
#6844 = VERTEX_POINT ( 'NONE', #11582 ) ;
#6845 = AXIS2_PLACEMENT_3D ( 'NONE', #7042, #6201, #1546 ) ;
#6846 = DIRECTION ( 'NONE',  ( -1.000000000000000000, -0.000000000000000000, -0.000000000000000000 ) ) ;
#6847 = CARTESIAN_POINT ( 'NONE',  ( 1.500000000000000444, -17.35216073792428304, -17.71842311621547594 ) ) ;
#6848 = CARTESIAN_POINT ( 'NONE',  ( -14.76245309360481706, 5.834016798581969532, 6.857782953271941950E-17 ) ) ;
#6849 = VERTEX_POINT ( 'NONE', #3311 ) ;
#6850 = AXIS2_PLACEMENT_3D ( 'NONE', #9255, #876, #8340 ) ;
#6851 = CARTESIAN_POINT ( 'NONE',  ( 50.00005079999999680, 0.000000000000000000, 0.000000000000000000 ) ) ;
#6852 = CIRCLE ( 'NONE', #3348, 9.599999999999997868 ) ;
#6853 = CIRCLE ( 'NONE', #1586, 9.599999999999996092 ) ;
#6854 = DIRECTION ( 'NONE',  ( -1.000000000000000000, -0.000000000000000000, 0.000000000000000000 ) ) ;
#6855 = CIRCLE ( 'NONE', #605, 22.99900000000000233 ) ;
#6856 = VERTEX_POINT ( 'NONE', #372 ) ;
#6857 = CARTESIAN_POINT ( 'NONE',  ( 9.701579622838506722, -3.641351606116563389, 10.00000000000000000 ) ) ;
#6858 = CARTESIAN_POINT ( 'NONE',  ( 3.000000000000000888, 6.779701584703024864, -21.97702544527750845 ) ) ;
#6859 = CLOSED_SHELL ( 'NONE', ( #7119, #746, #4332, #7556, #4826, #11593 ) ) ;
#6861 = AXIS2_PLACEMENT_3D ( 'NONE', #11481, #9522, #9759 ) ;
#6860 = CARTESIAN_POINT ( 'NONE',  ( 0.000000000000000000, 0.000000000000000000, 0.000000000000000000 ) ) ;
#6862 = CARTESIAN_POINT ( 'NONE',  ( 3.000000000000000888, 0.000000000000000000, 0.000000000000000000 ) ) ;
#6863 = CARTESIAN_POINT ( 'NONE',  ( -12.91830213043054698, -2.344901317288422327, 10.00000000000000000 ) ) ;
#6864 = CIRCLE ( 'NONE', #2765, 24.80000000000000071 ) ;
#6865 = FACE_OUTER_BOUND ( 'NONE', #4437, .T. ) ;
#6866 = DIRECTION ( 'NONE',  ( 0.000000000000000000, 0.000000000000000000, 1.000000000000000000 ) ) ;
#6867 = LINE ( 'NONE', #5844, #10948 ) ;
#6868 = CIRCLE ( 'NONE', #4329, 9.599999999999997868 ) ;
#6869 = EDGE_LOOP ( 'NONE', ( #2675, #7272, #6984, #11942 ) ) ;
#6870 = EDGE_CURVE ( 'NONE', #2802, #401, #2464, .T. ) ;
#6871 = ORIENTED_EDGE ( 'NONE', *, *, #1520, .T. ) ;
#6872 = ORIENTED_EDGE ( 'NONE', *, *, #10097, .F. ) ;
#6873 = DIRECTION ( 'NONE',  ( -1.000000000000000000, -0.000000000000000000, 0.000000000000000000 ) ) ;
#6874 = CARTESIAN_POINT ( 'NONE',  ( 2.467392210070201486, 7.745125807189176648, 10.00000000000000000 ) ) ;
#6875 = EDGE_CURVE ( 'NONE', #10349, #10186, #10873, .T. ) ;
#6876 = DIRECTION ( 'NONE',  ( 1.000000000000000000, 0.000000000000000000, 0.000000000000000000 ) ) ;
#6877 = ADVANCED_FACE ( 'NONE', ( #3252 ), #6134, .T. ) ;
#6878 = CIRCLE ( 'NONE', #10204, 9.599999999999999645 ) ;
#6879 = CARTESIAN_POINT ( 'NONE',  ( 11.37845468071832222, 2.456417158213071161, 10.00000000000000000 ) ) ;
#6880 = CIRCLE ( 'NONE', #1616, 22.00000000000000000 ) ;
#6881 = CARTESIAN_POINT ( 'NONE',  ( -16.06046882360139350, -0.5196555361422402486, 6.857782953271941950E-17 ) ) ;
#6882 = EDGE_CURVE ( 'NONE', #6658, #8357, #11644, .T. ) ;
#6883 = CARTESIAN_POINT ( 'NONE',  ( 0.000000000000000000, -17.71842311621518462, -17.35216073792458857 ) ) ;
#6884 = DIRECTION ( 'NONE',  ( 0.000000000000000000, 0.000000000000000000, 1.000000000000000000 ) ) ;
#6885 = VERTEX_POINT ( 'NONE', #9800 ) ;
#6886 = ORIENTED_EDGE ( 'NONE', *, *, #5957, .F. ) ;
#6887 = ORIENTED_EDGE ( 'NONE', *, *, #3040, .T. ) ;
#6888 = CARTESIAN_POINT ( 'NONE',  ( 3.000000000000000888, -16.85990652506889376, -15.64281154287614584 ) ) ;
#6889 = AXIS2_PLACEMENT_3D ( 'NONE', #9400, #10199, #33 ) ;
#6890 = CARTESIAN_POINT ( 'NONE',  ( 3.000000000000000888, 0.000000000000000000, 0.000000000000000000 ) ) ;
#6891 = CARTESIAN_POINT ( 'NONE',  ( 3.000000000000000000, 0.000000000000000000, 0.000000000000000000 ) ) ;
#6892 = VECTOR ( 'NONE', #10607, 1000.000000000000000 ) ;
#6893 = DIRECTION ( 'NONE',  ( 0.000000000000000000, -0.7431448254773862505, -0.6691306063588672304 ) ) ;
#6894 = CARTESIAN_POINT ( 'NONE',  ( -8.984113827416486231, -1.502549133976348372, 3.747395293195558847E-16 ) ) ;
#6895 = FACE_OUTER_BOUND ( 'NONE', #6352, .T. ) ;
#6896 = VERTEX_POINT ( 'NONE', #8888 ) ;
#6897 = ORIENTED_EDGE ( 'NONE', *, *, #8826, .T. ) ;
#6898 = EDGE_CURVE ( 'NONE', #1562, #6584, #5394, .T. ) ;
#6899 = DIRECTION ( 'NONE',  ( 0.000000000000000000, 0.000000000000000000, 1.000000000000000000 ) ) ;
#6900 = CARTESIAN_POINT ( 'NONE',  ( 7.619603487155713673, -11.82824555707897218, 10.00000000000000000 ) ) ;
#6901 = ORIENTED_EDGE ( 'NONE', *, *, #444, .T. ) ;
#6902 = CARTESIAN_POINT ( 'NONE',  ( 22.00000000000000000, 2.694222958124176809E-15, 20.00000000000000000 ) ) ;
#6903 = FACE_OUTER_BOUND ( 'NONE', #8571, .T. ) ;
#6904 = EDGE_CURVE ( 'NONE', #10278, #1309, #9690, .T. ) ;
#6905 = AXIS2_PLACEMENT_3D ( 'NONE', #8817, #7765, #1285 ) ;
#6906 = DIRECTION ( 'NONE',  ( -1.000000000000000000, 0.000000000000000000, 0.000000000000000000 ) ) ;
#6907 = ORIENTED_EDGE ( 'NONE', *, *, #2288, .F. ) ;
#6908 = CARTESIAN_POINT ( 'NONE',  ( 3.000000000000000888, 3.623565124517435176, -24.53384959170454138 ) ) ;
#6909 = CARTESIAN_POINT ( 'NONE',  ( 3.000000000000000888, 15.42759117534385993, 16.45023496161670451 ) ) ;
#6910 = CARTESIAN_POINT ( 'NONE',  ( 6.986659217179107095, 9.748146710219840472, 6.857782953271941950E-17 ) ) ;
#6911 = VERTEX_POINT ( 'NONE', #3379 ) ;
#6912 = EDGE_CURVE ( 'NONE', #10809, #5848, #6430, .T. ) ;
#6913 = CARTESIAN_POINT ( 'NONE',  ( 0.000000000000000000, -13.28910708463113721, -20.93895013827595264 ) ) ;
#6914 = CIRCLE ( 'NONE', #460, 24.80000000000000071 ) ;
#6915 = DIRECTION ( 'NONE',  ( 0.000000000000000000, 0.7431448254773955764, -0.6691306063588569053 ) ) ;
#6916 = VERTEX_POINT ( 'NONE', #680 ) ;
#6917 = CARTESIAN_POINT ( 'NONE',  ( -4.622662292628551661, -8.344572748942844953, 10.00000000000000000 ) ) ;
#6918 = DIRECTION ( 'NONE',  ( -1.000000000000000000, 0.000000000000000000, 0.000000000000000000 ) ) ;
#6919 = AXIS2_PLACEMENT_3D ( 'NONE', #10902, #8148, #11819 ) ;
#6920 = CARTESIAN_POINT ( 'NONE',  ( 0.000000000000000000, -17.35216073792452107, 17.71842311621524146 ) ) ;
#6921 = EDGE_CURVE ( 'NONE', #3750, #4226, #4411, .T. ) ;
#6922 = CYLINDRICAL_SURFACE ( 'NONE', #4979, 9.599999999999997868 ) ;
#6923 = CARTESIAN_POINT ( 'NONE',  ( 14.27634331491212549, 3.322769473269123974, 10.00000000000000000 ) ) ;
#6924 = LINE ( 'NONE', #9986, #8248 ) ;
#6925 = CYLINDRICAL_SURFACE ( 'NONE', #3977, 22.99899999999999878 ) ;
#6926 = CARTESIAN_POINT ( 'NONE',  ( 3.000000000000000888, 0.000000000000000000, 0.000000000000000000 ) ) ;
#6927 = VERTEX_POINT ( 'NONE', #798 ) ;
#6928 = DIRECTION ( 'NONE',  ( 0.000000000000000000, -0.3090169943749349057, -0.9510565162951577500 ) ) ;
#6929 = ORIENTED_EDGE ( 'NONE', *, *, #4263, .F. ) ;
#6930 = CARTESIAN_POINT ( 'NONE',  ( -2.958039891549808509, 0.5000000000000001110, 0.000000000000000000 ) ) ;
#6931 = CARTESIAN_POINT ( 'NONE',  ( 3.000000000000000888, 0.000000000000000000, 0.000000000000000000 ) ) ;
#6932 = LINE ( 'NONE', #2413, #6141 ) ;
#6933 = CARTESIAN_POINT ( 'NONE',  ( -5.125696908148163367, -9.212757455310160992, 10.00000000000000000 ) ) ;
#6934 = AXIS2_PLACEMENT_3D ( 'NONE', #7971, #11705, #11595 ) ;
#6935 = CARTESIAN_POINT ( 'NONE',  ( -15.85416723795448846, 2.087521067385502693, 6.857782953271941950E-17 ) ) ;
#6936 = FACE_OUTER_BOUND ( 'NONE', #6082, .T. ) ;
#6937 = CARTESIAN_POINT ( 'NONE',  ( 3.000000000000000888, 2.062268319295562424, 22.90635393027947231 ) ) ;
#6938 = ORIENTED_EDGE ( 'NONE', *, *, #9304, .F. ) ;
#6939 = VERTEX_POINT ( 'NONE', #10842 ) ;
#6940 = EDGE_CURVE ( 'NONE', #6916, #6856, #3640, .T. ) ;
#6941 = EDGE_LOOP ( 'NONE', ( #1754, #11020, #10365, #2623 ) ) ;
#6942 = CARTESIAN_POINT ( 'NONE',  ( 6.600721363681033793, -14.58171973507987751, 10.00000000000000000 ) ) ;
#6943 = ADVANCED_FACE ( 'NONE', ( #11870 ), #4540, .T. ) ;
#6944 = CARTESIAN_POINT ( 'NONE',  ( 0.000000000000000000, 0.000000000000000000, 0.000000000000000000 ) ) ;
#6945 = CARTESIAN_POINT ( 'NONE',  ( 8.000000000000000000, 0.000000000000000000, 0.000000000000000000 ) ) ;
#6946 = CARTESIAN_POINT ( 'NONE',  ( -6.597323627731391582, 9.514359934151556786, 3.747395293195558847E-16 ) ) ;
#6947 = CIRCLE ( 'NONE', #9897, 24.80000000000000071 ) ;
#6948 = EDGE_CURVE ( 'NONE', #490, #8778, #5979, .T. ) ;
#6949 = CARTESIAN_POINT ( 'NONE',  ( 3.000000000000000888, -7.402892494506152943, -21.30300407174369681 ) ) ;
#6950 = EDGE_LOOP ( 'NONE', ( #3621, #6396 ) ) ;
#6951 = ORIENTED_EDGE ( 'NONE', *, *, #1621, .F. ) ;
#6952 = CARTESIAN_POINT ( 'NONE',  ( 0.000000000000000000, 0.000000000000000000, 0.000000000000000000 ) ) ;
#6953 = CARTESIAN_POINT ( 'NONE',  ( -10.47176928358605075, -8.303818807687077808, 10.00000000000000000 ) ) ;
#6954 = ORIENTED_EDGE ( 'NONE', *, *, #4438, .F. ) ;
#6955 = DIRECTION ( 'NONE',  ( -1.000000000000000000, 0.000000000000000000, 0.000000000000000000 ) ) ;
#6956 = CARTESIAN_POINT ( 'NONE',  ( 3.000000000000000888, 0.000000000000000000, 0.000000000000000000 ) ) ;
#6957 = CARTESIAN_POINT ( 'NONE',  ( 3.000000000000000888, 0.4575788569254873317, -22.54798042742717712 ) ) ;
#6958 = AXIS2_PLACEMENT_3D ( 'NONE', #8070, #9163, #1701 ) ;
#6959 = ORIENTED_EDGE ( 'NONE', *, *, #8606, .F. ) ;
#6960 = DIRECTION ( 'NONE',  ( -1.000000000000000000, 0.000000000000000000, 0.000000000000000000 ) ) ;
#6961 = ADVANCED_FACE ( 'NONE', ( #10095 ), #8205, .T. ) ;
#6962 = DIRECTION ( 'NONE',  ( -1.000000000000000000, -0.000000000000000000, -0.000000000000000000 ) ) ;
#6963 = CARTESIAN_POINT ( 'NONE',  ( 10.54603994011982415, 5.199563424939647405, 6.857782953271941950E-17 ) ) ;
#6964 = ORIENTED_EDGE ( 'NONE', *, *, #1389, .T. ) ;
#6965 = ADVANCED_FACE ( 'NONE', ( #3500 ), #7334, .T. ) ;
#6966 = CARTESIAN_POINT ( 'NONE',  ( 0.000000000000000000, 19.10918332567958089, 15.80756504416697439 ) ) ;
#6967 = VERTEX_POINT ( 'NONE', #9004 ) ;
#6968 = CYLINDRICAL_SURFACE ( 'NONE', #4133, 22.99899999999999878 ) ;
#6969 = ORIENTED_EDGE ( 'NONE', *, *, #4943, .F. ) ;
#6970 = CARTESIAN_POINT ( 'NONE',  ( -11.92955594661033558, -2.174140050202246766, 10.00000000000000000 ) ) ;
#6971 = ORIENTED_EDGE ( 'NONE', *, *, #8542, .F. ) ;
#6972 = DIRECTION ( 'NONE',  ( 0.000000000000000000, 0.4067366430758009299, -0.9135454576426005335 ) ) ;
#6973 = SURFACE_STYLE_USAGE ( .BOTH. , #1355 ) ;
#6974 = ORIENTED_EDGE ( 'NONE', *, *, #9281, .T. ) ;
#6975 = CARTESIAN_POINT ( 'NONE',  ( 0.000000000000000000, -6.779701584702581663, -21.97702544527764701 ) ) ;
#6976 = LINE ( 'NONE', #11085, #2831 ) ;
#6977 = CARTESIAN_POINT ( 'NONE',  ( -2.433178163897189883, 9.086443520544605690, 10.00000000000000000 ) ) ;
#6978 = AXIS2_PLACEMENT_3D ( 'NONE', #7416, #8410, #9381 ) ;
#6979 = CARTESIAN_POINT ( 'NONE',  ( 3.000000000000000888, -24.53384959170455204, -3.623565124517360569 ) ) ;
#6980 = CARTESIAN_POINT ( 'NONE',  ( -6.777230418910821896, -10.52530689671158193, 3.747395293195558847E-16 ) ) ;
#6981 = EDGE_CURVE ( 'NONE', #2610, #10797, #2452, .T. ) ;
#6982 = CARTESIAN_POINT ( 'NONE',  ( 3.000000000000000888, -15.40502424595132247, -19.43515443678418819 ) ) ;
#6983 = DIRECTION ( 'NONE',  ( -1.000000000000000000, -0.000000000000000000, 0.000000000000000000 ) ) ;
#6984 = ORIENTED_EDGE ( 'NONE', *, *, #9761, .F. ) ;
#6985 = VECTOR ( 'NONE', #3876, 1000.000000000000000 ) ;
#6986 = CYLINDRICAL_SURFACE ( 'NONE', #896, 24.80000000000000071 ) ;
#6987 = VERTEX_POINT ( 'NONE', #6252 ) ;
#6988 = EDGE_CURVE ( 'NONE', #11921, #11607, #10476, .T. ) ;
#6989 = FACE_OUTER_BOUND ( 'NONE', #2129, .T. ) ;
#6990 = CARTESIAN_POINT ( 'NONE',  ( 3.000000000000000000, 2.265596578422603002E-15, -18.49999999999999645 ) ) ;
#6991 = CARTESIAN_POINT ( 'NONE',  ( -6.825012239887744414, 1.243808647927287403, 10.00000000000000000 ) ) ;
#6992 = CARTESIAN_POINT ( 'NONE',  ( -10.03906249502028558, -0.8181230654450031281, 6.857782953271941950E-17 ) ) ;
#6993 = AXIS2_PLACEMENT_3D ( 'NONE', #3792, #7513, #10326 ) ;
#6994 = CARTESIAN_POINT ( 'NONE',  ( 3.000000000000000888, -6.668524164681463695, -23.88662356770122130 ) ) ;
#6995 = ORIENTED_EDGE ( 'NONE', *, *, #8688, .F. ) ;
#6996 = AXIS2_PLACEMENT_3D ( 'NONE', #3592, #9150, #2613 ) ;
#6997 = EDGE_LOOP ( 'NONE', ( #7121, #9899, #11153, #10743 ) ) ;
#6998 = ORIENTED_EDGE ( 'NONE', *, *, #10919, .F. ) ;
#6999 = CARTESIAN_POINT ( 'NONE',  ( 1.499999999999999556, -24.75110766671651064, -1.556492618230889580 ) ) ;
#7000 = CARTESIAN_POINT ( 'NONE',  ( 0.000000000000000000, -13.72351598154911478, 20.65684170206487025 ) ) ;
#7001 = CARTESIAN_POINT ( 'NONE',  ( 0.000000000000000000, 18.80635025205170052, 13.23915371906961802 ) ) ;
#7002 = CARTESIAN_POINT ( 'NONE',  ( -8.111627617515257072, 3.498804908652022316, 3.747395293195558847E-16 ) ) ;
#7003 = DIRECTION ( 'NONE',  ( -1.000000000000000000, 0.000000000000000000, 0.000000000000000000 ) ) ;
#7004 = EDGE_CURVE ( 'NONE', #1445, #3234, #2514, .T. ) ;
#7005 = EDGE_CURVE ( 'NONE', #9959, #1167, #7151, .T. ) ;
#7006 = CYLINDRICAL_SURFACE ( 'NONE', #6636, 9.599999999999997868 ) ;
#7007 = VECTOR ( 'NONE', #4643, 1000.000000000000000 ) ;
#7008 = ORIENTED_EDGE ( 'NONE', *, *, #9874, .T. ) ;
#7009 = EDGE_LOOP ( 'NONE', ( #5189, #2484, #6995, #10973 ) ) ;
#7010 = CARTESIAN_POINT ( 'NONE',  ( 5.564773995946421969, -12.83798980516408683, 10.00000000000000000 ) ) ;
#7011 = VERTEX_POINT ( 'NONE', #1602 ) ;
#7012 = EDGE_CURVE ( 'NONE', #110, #9064, #7344, .T. ) ;
#7013 = CARTESIAN_POINT ( 'NONE',  ( 0.000000000000000000, 0.000000000000000000, 0.000000000000000000 ) ) ;
#7014 = CYLINDRICAL_SURFACE ( 'NONE', #4364, 18.49999999999999645 ) ;
#7015 = CARTESIAN_POINT ( 'NONE',  ( 3.000000000000000888, 22.56530478845649057, 4.445336973060936891 ) ) ;
#7016 = ORIENTED_EDGE ( 'NONE', *, *, #1168, .T. ) ;
#7018 = EDGE_CURVE ( 'NONE', #7573, #7873, #8342, .T. ) ;
#7017 = CIRCLE ( 'NONE', #6449, 24.80000000000000071 ) ;
#7019 = CARTESIAN_POINT ( 'NONE',  ( 0.000000000000000000, 0.000000000000000000, 0.000000000000000000 ) ) ;
#7020 = EDGE_CURVE ( 'NONE', #4653, #8232, #3462, .T. ) ;
#7021 = AXIS2_PLACEMENT_3D ( 'NONE', #9813, #745, #6146 ) ;
#7022 = LINE ( 'NONE', #10769, #6681 ) ;
#7023 = CARTESIAN_POINT ( 'NONE',  ( 2.469054641153893837, -10.61194774715159284, 6.857782953271941950E-17 ) ) ;
#7024 = EDGE_CURVE ( 'NONE', #4404, #67, #7937, .T. ) ;
#7025 = ORIENTED_EDGE ( 'NONE', *, *, #11435, .F. ) ;
#7026 = DIRECTION ( 'NONE',  ( 0.000000000000000000, 0.1045284632676538872, -0.9945218953682732899 ) ) ;
#7027 = DIRECTION ( 'NONE',  ( -1.000000000000000000, -0.000000000000000000, 0.000000000000000000 ) ) ;
#7028 = AXIS2_PLACEMENT_3D ( 'NONE', #1071, #3880, #7603 ) ;
#7029 = EDGE_LOOP ( 'NONE', ( #10532, #2483, #6161, #7780 ) ) ;
#7030 = CARTESIAN_POINT ( 'NONE',  ( 8.913847851856345983, -5.129921849437908854, 10.00000000000000000 ) ) ;
#7031 = AXIS2_PLACEMENT_3D ( 'NONE', #10531, #6738, #6915 ) ;
#7032 = ORIENTED_EDGE ( 'NONE', *, *, #5328, .T. ) ;
#7033 = CARTESIAN_POINT ( 'NONE',  ( 0.000000000000000000, -8.753070780933295936, 20.78471918669858098 ) ) ;
#7034 = LINE ( 'NONE', #10783, #11704 ) ;
#7035 = ORIENTED_EDGE ( 'NONE', *, *, #4897, .T. ) ;
#7036 = CYLINDRICAL_SURFACE ( 'NONE', #5044, 5.000000000000000000 ) ;
#7037 = DIRECTION ( 'NONE',  ( -1.000000000000000000, -0.000000000000000000, 0.000000000000000000 ) ) ;
#7038 = CARTESIAN_POINT ( 'NONE',  ( -0.8869411547437835441, -7.669649013129178350, 10.00000000000000000 ) ) ;
#7039 = DIRECTION ( 'NONE',  ( -1.000000000000000000, 0.000000000000000000, 0.000000000000000000 ) ) ;
#7040 = CARTESIAN_POINT ( 'NONE',  ( 13.54728169684850059, 0.8932250400879224728, 3.747395293195558847E-16 ) ) ;
#7041 = CARTESIAN_POINT ( 'NONE',  ( 0.000000000000000000, 10.87771529938188486, -19.75591328264875202 ) ) ;
#7042 = CARTESIAN_POINT ( 'NONE',  ( 3.000000000000000888, 0.000000000000000000, 0.000000000000000000 ) ) ;
#7043 = EDGE_LOOP ( 'NONE', ( #11782, #9472, #3072, #1612 ) ) ;
#7044 = CIRCLE ( 'NONE', #5102, 24.80000000000000071 ) ;
#7045 = DIRECTION ( 'NONE',  ( 3.469446951953614189E-16, 0.000000000000000000, 1.000000000000000000 ) ) ;
#7046 = ORIENTED_EDGE ( 'NONE', *, *, #1865, .F. ) ;
#7047 = VECTOR ( 'NONE', #8043, 1000.000000000000000 ) ;
#7048 = EDGE_CURVE ( 'NONE', #1491, #10316, #6666, .T. ) ;
#7049 = FACE_OUTER_BOUND ( 'NONE', #2387, .T. ) ;
#7050 = DIRECTION ( 'NONE',  ( 0.000000000000000000, 0.000000000000000000, 1.000000000000000000 ) ) ;
#7051 = DIRECTION ( 'NONE',  ( -0.000000000000000000, -0.000000000000000000, -1.000000000000000000 ) ) ;
#7052 = CARTESIAN_POINT ( 'NONE',  ( -7.014275365397510065, 0.1192422097806477982, 10.00000000000000000 ) ) ;
#7053 = CARTESIAN_POINT ( 'NONE',  ( 0.6097887191948974106, 9.229167205757265791, 6.857782953271941950E-17 ) ) ;
#7054 = FILL_AREA_STYLE_COLOUR ( '', #11204 ) ;
#7055 = LINE ( 'NONE', #10808, #8444 ) ;
#7056 = EDGE_LOOP ( 'NONE', ( #1530, #9422 ) ) ;
#7057 = EDGE_CURVE ( 'NONE', #5430, #8902, #5817, .T. ) ;
#7058 = AXIS2_PLACEMENT_3D ( 'NONE', #7144, #427, #1527 ) ;
#7059 = VERTEX_POINT ( 'NONE', #8391 ) ;
#7060 = ORIENTED_EDGE ( 'NONE', *, *, #11305, .T. ) ;
#7061 = CARTESIAN_POINT ( 'NONE',  ( -9.045553118584756191, -8.482981269325438944, 10.00000000000000000 ) ) ;
#7062 = AXIS2_PLACEMENT_3D ( 'NONE', #4042, #1287, #2142 ) ;
#7063 = FACE_OUTER_BOUND ( 'NONE', #11219, .T. ) ;
#7064 = DIRECTION ( 'NONE',  ( -1.000000000000000000, -0.000000000000000000, 0.000000000000000000 ) ) ;
#7065 = CIRCLE ( 'NONE', #4939, 22.99899999999999523 ) ;
#7066 = CARTESIAN_POINT ( 'NONE',  ( -3.516813791735896810, 7.717845097288992484, 3.747395293195558847E-16 ) ) ;
#7067 = DIRECTION ( 'NONE',  ( -1.000000000000000000, -0.000000000000000000, 0.000000000000000000 ) ) ;
#7068 = DIRECTION ( 'NONE',  ( -1.000000000000000000, -0.000000000000000000, 0.000000000000000000 ) ) ;
#7069 = ORIENTED_EDGE ( 'NONE', *, *, #5160, .T. ) ;
#7070 = ORIENTED_EDGE ( 'NONE', *, *, #299, .F. ) ;
#7071 = CARTESIAN_POINT ( 'NONE',  ( -12.59589084681761229, 2.937805917057824789, 10.00000000000000000 ) ) ;
#7072 = ORIENTED_EDGE ( 'NONE', *, *, #11726, .F. ) ;
#7073 = DIRECTION ( 'NONE',  ( -1.000000000000000000, 0.000000000000000000, -0.000000000000000000 ) ) ;
#7074 = DIRECTION ( 'NONE',  ( 1.000000000000000000, 0.000000000000000000, 0.000000000000000000 ) ) ;
#7075 = CARTESIAN_POINT ( 'NONE',  ( 0.000000000000000000, 15.64281154287597353, 16.85990652506905363 ) ) ;
#7076 = PRODUCT_DEFINITION_CONTEXT ( 'detailed design', #1138, 'design' ) ;
#7077 = CARTESIAN_POINT ( 'NONE',  ( 3.000000000000000888, 19.74380051311539930, 11.79560690673879186 ) ) ;
#7078 = ORIENTED_EDGE ( 'NONE', *, *, #2920, .F. ) ;
#7079 = CIRCLE ( 'NONE', #1239, 9.599999999999996092 ) ;
#7080 = CARTESIAN_POINT ( 'NONE',  ( 0.000000000000000000, 22.54798042742717712, 0.4575788569255671012 ) ) ;
#7081 = DIRECTION ( 'NONE',  ( 0.000000000000000000, 0.000000000000000000, 1.000000000000000000 ) ) ;
#7082 = CARTESIAN_POINT ( 'NONE',  ( -4.368568794346921358, -9.638580752213396607, 6.857782953271941950E-17 ) ) ;
#7083 = ADVANCED_FACE ( 'NONE', ( #9307 ), #4778, .F. ) ;
#7084 = AXIS2_PLACEMENT_3D ( 'NONE', #4777, #8515, #11321 ) ;
#7085 = CARTESIAN_POINT ( 'NONE',  ( 3.000000000000000888, -21.76479567747246691, 7.432877647175128999 ) ) ;
#7086 = CARTESIAN_POINT ( 'NONE',  ( 0.07364157424580680678, -3.751631698233684364, 10.00000000000000000 ) ) ;
#7087 = VERTEX_POINT ( 'NONE', #4724 ) ;
#7088 = ADVANCED_FACE ( 'NONE', ( #12113 ), #8332, .T. ) ;
#7089 = CIRCLE ( 'NONE', #8677, 11.50000000000000178 ) ;
#7090 = CARTESIAN_POINT ( 'NONE',  ( -6.597323627732286866, 9.514359934152452070, 10.00000000000000000 ) ) ;
#7091 = EDGE_CURVE ( 'NONE', #8051, #7087, #922, .T. ) ;
#7092 = VERTEX_POINT ( 'NONE', #11140 ) ;
#7093 = DIRECTION ( 'NONE',  ( 0.000000000000000000, 0.000000000000000000, 1.000000000000000000 ) ) ;
#7094 = EDGE_LOOP ( 'NONE', ( #7928, #4969, #8953, #3394 ) ) ;
#7095 = EDGE_CURVE ( 'NONE', #35, #5430, #4818, .T. ) ;
#7096 = CARTESIAN_POINT ( 'NONE',  ( 0.000000000000000000, -22.15038895030646060, -4.240409074144325885 ) ) ;
#7097 = DIRECTION ( 'NONE',  ( -1.000000000000000000, 0.000000000000000000, 0.000000000000000000 ) ) ;
#7098 = CARTESIAN_POINT ( 'NONE',  ( -7.708066421255711731, 5.920849505456871498, 10.00000000000000000 ) ) ;
#7099 = CIRCLE ( 'NONE', #1839, 22.99899999999999878 ) ;
#7100 = CYLINDRICAL_SURFACE ( 'NONE', #8046, 22.99899999999999878 ) ;
#7101 = CARTESIAN_POINT ( 'NONE',  ( 12.96212312671852551, -3.473279994529273829, 3.747395293195558847E-16 ) ) ;
#7102 = CARTESIAN_POINT ( 'NONE',  ( 3.000000000000000888, 0.000000000000000000, 0.000000000000000000 ) ) ;
#7103 = ORIENTED_EDGE ( 'NONE', *, *, #9658, .F. ) ;
#7104 = DIRECTION ( 'NONE',  ( -1.000000000000000000, 0.000000000000000000, 0.000000000000000000 ) ) ;
#7105 = VERTEX_POINT ( 'NONE', #12054 ) ;
#7106 = ADVANCED_FACE ( 'NONE', ( #57 ), #8574, .T. ) ;
#7107 = DIRECTION ( 'NONE',  ( 0.000000000000000000, -0.5000000000000072164, 0.8660254037844345998 ) ) ;
#7108 = DIRECTION ( 'NONE',  ( -0.000000000000000000, -0.000000000000000000, 1.000000000000000000 ) ) ;
#7109 = SURFACE_STYLE_USAGE ( .BOTH. , #6333 ) ;
#7110 = ORIENTED_EDGE ( 'NONE', *, *, #2922, .T. ) ;
#7111 = CARTESIAN_POINT ( 'NONE',  ( 8.000000000000000000, 0.000000000000000000, 18.49999999999999645 ) ) ;
#7112 = DIRECTION ( 'NONE',  ( 1.000000000000000000, 0.000000000000000000, 0.000000000000000000 ) ) ;
#7113 = CARTESIAN_POINT ( 'NONE',  ( 3.000000000000000888, -19.10918332567947076, -15.80756504416710229 ) ) ;
#7114 = EDGE_CURVE ( 'NONE', #6489, #3556, #912, .T. ) ;
#7115 = CARTESIAN_POINT ( 'NONE',  ( 9.774996403550728630, -5.644905071530503804, 6.857782953271941950E-17 ) ) ;
#7116 = AXIS2_PLACEMENT_3D ( 'NONE', #3444, #5520, #738 ) ;
#7117 = CARTESIAN_POINT ( 'NONE',  ( 0.000000000000000000, -18.40266524480579236, -13.79477846460815194 ) ) ;
#7118 = VERTEX_POINT ( 'NONE', #1103 ) ;
#7119 = ADVANCED_FACE ( 'NONE', ( #11322 ), #4659, .T. ) ;
#7120 = EDGE_LOOP ( 'NONE', ( #7744, #7980, #6192, #10727 ) ) ;
#7121 = ORIENTED_EDGE ( 'NONE', *, *, #767, .T. ) ;
#7122 = EDGE_CURVE ( 'NONE', #4609, #6489, #6574, .T. ) ;
#7123 = CARTESIAN_POINT ( 'NONE',  ( -1.035167565893234443, -12.71157708251009488, 10.00000000000000000 ) ) ;
#7124 = CARTESIAN_POINT ( 'NONE',  ( 3.000000000000000888, 2.745295967525994918, 22.83456483164690098 ) ) ;
#7125 = DIRECTION ( 'NONE',  ( 0.000000000000000000, 0.000000000000000000, 1.000000000000000000 ) ) ;
#7126 = ADVANCED_FACE ( 'NONE', ( #5760 ), #6605, .T. ) ;
#7127 = CARTESIAN_POINT ( 'NONE',  ( 1.482756436301464920, -6.713508106970949463, 3.747395293195558847E-16 ) ) ;
#7128 = CARTESIAN_POINT ( 'NONE',  ( 0.000000000000000000, 0.000000000000000000, 0.000000000000000000 ) ) ;
#7129 = CYLINDRICAL_SURFACE ( 'NONE', #2141, 9.599999999999997868 ) ;
#7130 = ORIENTED_EDGE ( 'NONE', *, *, #9751, .F. ) ;
#7131 = ORIENTED_EDGE ( 'NONE', *, *, #4834, .T. ) ;
#7132 = AXIS2_PLACEMENT_3D ( 'NONE', #8847, #2287, #9695 ) ;
#7133 = EDGE_LOOP ( 'NONE', ( #3902, #8113 ) ) ;
#7134 = CARTESIAN_POINT ( 'NONE',  ( -4.491015865170432164, 3.510096388331073403, 10.00000000000000000 ) ) ;
#7135 = CARTESIAN_POINT ( 'NONE',  ( 3.000000000000000888, 20.86861857134734421, 9.667200211209893368 ) ) ;
#7136 = DIRECTION ( 'NONE',  ( 0.000000000000000000, 0.9945218953682737340, -0.1045284632676502651 ) ) ;
#7137 = DIRECTION ( 'NONE',  ( -1.000000000000000000, 0.000000000000000000, -0.000000000000000000 ) ) ;
#7138 = ORIENTED_EDGE ( 'NONE', *, *, #4953, .T. ) ;
#7139 = EDGE_CURVE ( 'NONE', #5674, #12055, #11210, .T. ) ;
#7140 = DIRECTION ( 'NONE',  ( 0.000000000000000000, -0.4999999999999887867, -0.8660254037844449249 ) ) ;
#7141 = AXIS2_PLACEMENT_3D ( 'NONE', #10353, #8654, #4739 ) ;
#7142 = CARTESIAN_POINT ( 'NONE',  ( 3.000000000000000888, 5.135568396240030253, 21.96011696265493285 ) ) ;
#7143 = CARTESIAN_POINT ( 'NONE',  ( -9.650762677556027569, -3.270672451565358685, 6.857782953271941950E-17 ) ) ;
#7144 = CARTESIAN_POINT ( 'NONE',  ( 0.000000000000000000, -0.4575788569253416149, 22.54798042742717712 ) ) ;
#7145 = CYLINDRICAL_SURFACE ( 'NONE', #9596, 9.599999999999997868 ) ;
#7146 = EDGE_LOOP ( 'NONE', ( #8855, #1898, #5990, #7808 ) ) ;
#7147 = ORIENTED_EDGE ( 'NONE', *, *, #2427, .F. ) ;
#7148 = VECTOR ( 'NONE', #7644, 1000.000000000000000 ) ;
#7149 = CARTESIAN_POINT ( 'NONE',  ( -4.763935748647996959, -4.221771024092342728, 10.00000000000000000 ) ) ;
#7150 = VERTEX_POINT ( 'NONE', #9366 ) ;
#7151 = LINE ( 'NONE', #6193, #2871 ) ;
#7152 = EDGE_CURVE ( 'NONE', #5430, #10713, #5986, .T. ) ;
#7153 = CARTESIAN_POINT ( 'NONE',  ( -2.958039891549808953, -0.4999999999999997780, 3.000000000000000000 ) ) ;
#7154 = CARTESIAN_POINT ( 'NONE',  ( 0.000000000000000000, 0.000000000000000000, 0.000000000000000000 ) ) ;
#7155 = CARTESIAN_POINT ( 'NONE',  ( 7.449730884303676248, -3.679036338562946096, 10.00000000000000000 ) ) ;
#7156 = LINE ( 'NONE', #10668, #1801 ) ;
#7157 = CARTESIAN_POINT ( 'NONE',  ( 7.081399987883180813, -10.98142027556026612, 3.747395293195558847E-16 ) ) ;
#7158 = CARTESIAN_POINT ( 'NONE',  ( 3.000000000000000888, -4.445336973061013275, 22.56530478845647991 ) ) ;
#7159 = ORIENTED_EDGE ( 'NONE', *, *, #10840, .F. ) ;
#7160 = ADVANCED_FACE ( 'NONE', ( #1900 ), #2882, .T. ) ;
#7161 = ORIENTED_EDGE ( 'NONE', *, *, #8065, .F. ) ;
#7162 = EDGE_CURVE ( 'NONE', #6372, #1694, #1958, .T. ) ;
#7163 = DIRECTION ( 'NONE',  ( -1.000000000000000000, -0.000000000000000000, 0.000000000000000000 ) ) ;
#7164 = ORIENTED_EDGE ( 'NONE', *, *, #7867, .F. ) ;
#7165 = CARTESIAN_POINT ( 'NONE',  ( -2.296015608618632076, -6.188270089871726221, 3.747395293195558847E-16 ) ) ;
#7166 = CARTESIAN_POINT ( 'NONE',  ( 3.000000000000000888, -21.76479567747236743, -7.432877647175426539 ) ) ;
#7167 = SURFACE_STYLE_FILL_AREA ( #3400 ) ;
#7168 = ORIENTED_EDGE ( 'NONE', *, *, #466, .T. ) ;
#7169 = CIRCLE ( 'NONE', #729, 24.80000000000000071 ) ;
#7170 = DIRECTION ( 'NONE',  ( 0.000000000000000000, 0.000000000000000000, 1.000000000000000000 ) ) ;
#7171 = CARTESIAN_POINT ( 'NONE',  ( 3.000000000000000888, -20.41249101028218149, 9.589108953447823325 ) ) ;
#7172 = DIRECTION ( 'NONE',  ( 0.000000000000000000, -0.9135454576425964257, -0.4067366430758103668 ) ) ;
#7173 = CARTESIAN_POINT ( 'NONE',  ( -0.5113267480521390684, 6.289062763288780999, 10.00000000000000000 ) ) ;
#7174 = EDGE_CURVE ( 'NONE', #9646, #9620, #7746, .T. ) ;
#7175 = CARTESIAN_POINT ( 'NONE',  ( 11.37845468071831512, 2.456417158213069829, 6.857782953271941950E-17 ) ) ;
#7176 = CARTESIAN_POINT ( 'NONE',  ( 8.000000000000000000, 0.000000000000000000, 18.49999999999999645 ) ) ;
#7177 = ADVANCED_FACE ( 'NONE', ( #5877 ), #2201, .T. ) ;
#7178 = CARTESIAN_POINT ( 'NONE',  ( 7.228014483236684722E-17, -0.4999999999999993339, 3.000000000000000000 ) ) ;
#7179 = EDGE_LOOP ( 'NONE', ( #2600, #6811, #809, #3440 ) ) ;
#7180 = ORIENTED_EDGE ( 'NONE', *, *, #3112, .F. ) ;
#7181 = CARTESIAN_POINT ( 'NONE',  ( -11.62103867303406979, 2.700230667072889279, 10.00000000000000000 ) ) ;
#7182 = LINE ( 'NONE', #6221, #6031 ) ;
#7183 = CARTESIAN_POINT ( 'NONE',  ( 0.000000000000000000, -23.88662356770119644, 6.668524164681547184 ) ) ;
#7184 = CIRCLE ( 'NONE', #7970, 9.599999999999997868 ) ;
#7185 = EDGE_CURVE ( 'NONE', #4549, #3254, #5942, .T. ) ;
#7186 = CARTESIAN_POINT ( 'NONE',  ( -5.541928854458315179, -2.884958602215172085, 3.747395293195558847E-16 ) ) ;
#7187 = CARTESIAN_POINT ( 'NONE',  ( 3.000000000000000888, 6.779701584702736206, 21.97702544527760082 ) ) ;
#7188 = LINE ( 'NONE', #11004, #8984 ) ;
#7189 = ORIENTED_EDGE ( 'NONE', *, *, #7004, .F. ) ;
#7190 = ORIENTED_EDGE ( 'NONE', *, *, #3339, .F. ) ;
#7191 = VERTEX_POINT ( 'NONE', #6052 ) ;
#7192 = DIRECTION ( 'NONE',  ( 0.000000000000000000, 0.4999999999999950040, 0.8660254037844415942 ) ) ;
#7193 = AXIS2_PLACEMENT_3D ( 'NONE', #236, #3981, #417 ) ;
#7194 = CIRCLE ( 'NONE', #1537, 22.99899999999999878 ) ;
#7195 = CARTESIAN_POINT ( 'NONE',  ( 3.000000000000000888, 0.000000000000000000, 0.000000000000000000 ) ) ;
#7196 = UNCERTAINTY_MEASURE_WITH_UNIT (LENGTH_MEASURE( 1.000000000000000082E-05 ), #3634, 'distance_accuracy_value', 'NONE');
#7197 = CARTESIAN_POINT ( 'NONE',  ( -10.00000000000000000, 0.000000000000000000, 0.000000000000000000 ) ) ;
#7198 = VERTEX_POINT ( 'NONE', #4164 ) ;
#7199 = EDGE_CURVE ( 'NONE', #4173, #9819, #318, .T. ) ;
#7200 = DIRECTION ( 'NONE',  ( -1.000000000000000000, -0.000000000000000000, -0.000000000000000000 ) ) ;
#7201 = DIRECTION ( 'NONE',  ( 0.000000000000000000, 0.000000000000000000, -1.000000000000000000 ) ) ;
#7202 = CARTESIAN_POINT ( 'NONE',  ( -6.829322889802579510, -2.192323464439260849, 6.857782953271941950E-17 ) ) ;
#7203 = AXIS2_PLACEMENT_3D ( 'NONE', #9961, #11912, #1582 ) ;
#7204 = CIRCLE ( 'NONE', #1941, 9.599999999999999645 ) ;
#7205 = DIRECTION ( 'NONE',  ( 0.000000000000000000, 0.000000000000000000, 1.000000000000000000 ) ) ;
#7206 = DIRECTION ( 'NONE',  ( 1.000000000000000000, 0.000000000000000000, 0.000000000000000000 ) ) ;
#7207 = EDGE_CURVE ( 'NONE', #1101, #10684, #8736, .T. ) ;
#7208 = ORIENTED_EDGE ( 'NONE', *, *, #10122, .F. ) ;
#7209 = ORIENTED_EDGE ( 'NONE', *, *, #2385, .F. ) ;
#7210 = CARTESIAN_POINT ( 'NONE',  ( 0.8073695008816145213, 5.181225205791319510, 10.00000000000000000 ) ) ;
#7211 = AXIS2_PLACEMENT_3D ( 'NONE', #908, #2004, #965 ) ;
#7212 = VERTEX_POINT ( 'NONE', #355 ) ;
#7213 = CARTESIAN_POINT ( 'NONE',  ( 0.000000000000000000, 0.000000000000000000, 0.000000000000000000 ) ) ;
#7214 = EDGE_LOOP ( 'NONE', ( #10263, #3573, #8990, #12092 ) ) ;
#7215 = AXIS2_PLACEMENT_3D ( 'NONE', #6597, #6717, #10453 ) ;
#7216 = DIRECTION ( 'NONE',  ( 0.000000000000000000, 0.000000000000000000, 1.000000000000000000 ) ) ;
#7217 = CARTESIAN_POINT ( 'NONE',  ( 1.499999999999999556, -1.556492618230471692, -24.75110766671653906 ) ) ;
#7218 = CARTESIAN_POINT ( 'NONE',  ( 8.539395351299297943, 0.2748098766782894331, 10.00000000000000000 ) ) ;
#7219 = DIRECTION ( 'NONE',  ( -1.000000000000000000, 0.000000000000000000, 0.000000000000000000 ) ) ;
#7220 = AXIS2_PLACEMENT_3D ( 'NONE', #9144, #9389, #1736 ) ;
#7221 = CARTESIAN_POINT ( 'NONE',  ( 0.000000000000000000, 22.54798042742718067, -0.4575788569252652871 ) ) ;
#7222 = ORIENTED_EDGE ( 'NONE', *, *, #3523, .F. ) ;
#7223 = CARTESIAN_POINT ( 'NONE',  ( 11.50000000000000178, 1.408343819019456373E-15, 4.000000000000000000 ) ) ;
#7224 = CIRCLE ( 'NONE', #9388, 24.80000000000000071 ) ;
#7225 = ORIENTED_EDGE ( 'NONE', *, *, #361, .T. ) ;
#7226 = CARTESIAN_POINT ( 'NONE',  ( 2.581500635392914411, -6.456130005640034142, 3.747395293195558847E-16 ) ) ;
#7227 = CARTESIAN_POINT ( 'NONE',  ( -10.00000000000000000, 0.000000000000000000, 0.000000000000000000 ) ) ;
#7228 = EDGE_LOOP ( 'NONE', ( #5332, #2246, #11082, #9374 ) ) ;
#7229 = DIRECTION ( 'NONE',  ( 1.000000000000000000, 0.000000000000000000, 0.000000000000000000 ) ) ;
#7230 = AXIS2_PLACEMENT_3D ( 'NONE', #5507, #7572, #5868 ) ;
#7231 = CARTESIAN_POINT ( 'NONE',  ( 0.000000000000000000, 0.000000000000000000, 0.000000000000000000 ) ) ;
#7232 = CARTESIAN_POINT ( 'NONE',  ( -2.061894914253513456, 6.087690860853038899, 10.00000000000000000 ) ) ;
#7233 = CARTESIAN_POINT ( 'NONE',  ( 5.508953106497944674, 1.454581011951804559, 6.857782953271941950E-17 ) ) ;
#7234 = AXIS2_PLACEMENT_3D ( 'NONE', #6952, #1220, #1099 ) ;
#7235 = CARTESIAN_POINT ( 'NONE',  ( 0.000000000000000000, 13.72351598154897268, 20.65684170206496262 ) ) ;
#7236 = DIRECTION ( 'NONE',  ( -1.000000000000000000, 0.000000000000000000, -0.000000000000000000 ) ) ;
#7237 = EDGE_CURVE ( 'NONE', #7440, #12091, #297, .T. ) ;
#7238 = ORIENTED_EDGE ( 'NONE', *, *, #5583, .F. ) ;
#7239 = AXIS2_PLACEMENT_3D ( 'NONE', #11245, #11057, #5670 ) ;
#7240 = AXIS2_PLACEMENT_3D ( 'NONE', #10414, #6004, #9495 ) ;
#7241 = ORIENTED_EDGE ( 'NONE', *, *, #9355, .T. ) ;
#7242 = CARTESIAN_POINT ( 'NONE',  ( -5.008276813248565773, -11.55791719732261669, 10.00000000000000000 ) ) ;
#7243 = ADVANCED_FACE ( 'NONE', ( #6782 ), #7890, .T. ) ;
#7244 = PLANE ( 'NONE',  #3692 ) ;
#7245 = DIRECTION ( 'NONE',  ( 0.000000000000000000, 1.000000000000000000, 3.491481338843133355E-15 ) ) ;
#7246 = CIRCLE ( 'NONE', #8801, 24.80000000000000071 ) ;
#7247 = CARTESIAN_POINT ( 'NONE',  ( -0.1586286459269546645, 8.284426055182338544, 3.747395293195558847E-16 ) ) ;
#7248 = CARTESIAN_POINT ( 'NONE',  ( 0.000000000000000000, 0.000000000000000000, 0.000000000000000000 ) ) ;
#7249 = DIRECTION ( 'NONE',  ( -1.000000000000000000, -0.000000000000000000, -0.000000000000000000 ) ) ;
#7250 = ORIENTED_EDGE ( 'NONE', *, *, #7955, .F. ) ;
#7251 = VERTEX_POINT ( 'NONE', #5071 ) ;
#7252 = ITEM_DEFINED_TRANSFORMATION ( 'NONE', 'NONE', #7234,  #8474 ) ;
#7253 = AXIS2_PLACEMENT_3D ( 'NONE', #8950, #3446, #8837 ) ;
#7254 = ORIENTED_EDGE ( 'NONE', *, *, #3326, .F. ) ;
#7255 = CARTESIAN_POINT ( 'NONE',  ( 8.000000000000000000, 2.449293598294706119E-15, -19.99999999999999645 ) ) ;
#7256 = AXIS2_PLACEMENT_3D ( 'NONE', #304, #11504, #3127 ) ;
#7257 = LINE ( 'NONE', #8988, #12101 ) ;
#7258 = LINE ( 'NONE', #11980, #3281 ) ;
#7259 = CARTESIAN_POINT ( 'NONE',  ( 0.000000000000000000, 0.000000000000000000, 0.000000000000000000 ) ) ;
#7260 = CARTESIAN_POINT ( 'NONE',  ( 3.000000000000000888, 11.67026512804547345, 19.29833442572363822 ) ) ;
#7261 = CARTESIAN_POINT ( 'NONE',  ( -3.764233030011069125, -6.516208816467297105, 6.857782953271941950E-17 ) ) ;
#7262 = CIRCLE ( 'NONE', #8259, 9.599999999999997868 ) ;
#7263 = EDGE_CURVE ( 'NONE', #9548, #11784, #7946, .T. ) ;
#7264 = CARTESIAN_POINT ( 'NONE',  ( 3.000000000000000888, 21.58580335785676496, 6.532525787311040943 ) ) ;
#7265 = VERTEX_POINT ( 'NONE', #3237 ) ;
#7266 = DIRECTION ( 'NONE',  ( -1.000000000000000000, -0.000000000000000000, 0.000000000000000000 ) ) ;
#7267 = ORIENTED_EDGE ( 'NONE', *, *, #5312, .F. ) ;
#7268 = EDGE_CURVE ( 'NONE', #5236, #6096, #6947, .T. ) ;
#7269 = ORIENTED_EDGE ( 'NONE', *, *, #10878, .F. ) ;
#7270 = CARTESIAN_POINT ( 'NONE',  ( -1.790740696106539520, -6.394195405909708363, 10.00000000000000000 ) ) ;
#7271 = CIRCLE ( 'NONE', #4762, 22.99899999999999523 ) ;
#7272 = ORIENTED_EDGE ( 'NONE', *, *, #2658, .F. ) ;
#7273 = DIRECTION ( 'NONE',  ( -1.000000000000000000, 0.000000000000000000, -0.000000000000000000 ) ) ;
#7274 = VERTEX_POINT ( 'NONE', #8637 ) ;
#7275 = DIRECTION ( 'NONE',  ( -1.000000000000000000, 0.000000000000000000, -0.000000000000000000 ) ) ;
#7276 = AXIS2_PLACEMENT_3D ( 'NONE', #5657, #9387, #5726 ) ;
#7277 = EDGE_CURVE ( 'NONE', #4353, #6571, #4963, .T. ) ;
#7278 = CARTESIAN_POINT ( 'NONE',  ( 3.000000000000000888, 0.000000000000000000, 0.000000000000000000 ) ) ;
#7279 = CARTESIAN_POINT ( 'NONE',  ( -6.661525743073271499, 1.789546221321743458, 10.00000000000000000 ) ) ;
#7280 = CARTESIAN_POINT ( 'NONE',  ( 3.000000000000000888, 0.4575788569251889593, 22.54798042742718067 ) ) ;
#7281 = DIRECTION ( 'NONE',  ( -1.000000000000000000, 0.000000000000000000, 0.000000000000000000 ) ) ;
#7282 = AXIS2_PLACEMENT_3D ( 'NONE', #2502, #4399, #3367 ) ;
#7283 = ORIENTED_EDGE ( 'NONE', *, *, #5617, .T. ) ;
#7284 = CARTESIAN_POINT ( 'NONE',  ( 3.000000000000000888, 5.117118920208487687, 22.42251312757881365 ) ) ;
#7285 = ORIENTED_EDGE ( 'NONE', *, *, #8539, .T. ) ;
#7286 = AXIS2_PLACEMENT_3D ( 'NONE', #7708, #11441, #477 ) ;
#7287 = CARTESIAN_POINT ( 'NONE',  ( 0.07364157424580704270, -3.751631698233870438, 3.747395293195558847E-16 ) ) ;
#7288 = CARTESIAN_POINT ( 'NONE',  ( 3.000000000000000888, -17.97274125076064877, -13.62355943574037731 ) ) ;
#7289 = ORIENTED_EDGE ( 'NONE', *, *, #5232, .T. ) ;
#7290 = AXIS2_PLACEMENT_3D ( 'NONE', #2349, #571, #1374 ) ;
#7291 = DIRECTION ( 'NONE',  ( -1.000000000000000000, 0.000000000000000000, -0.000000000000000000 ) ) ;
#7292 = CYLINDRICAL_SURFACE ( 'NONE', #1257, 22.99899999999999878 ) ;
#7293 = CARTESIAN_POINT ( 'NONE',  ( 14.52660474336370200, -9.366294961249359119, 10.00000000000000000 ) ) ;
#7294 = CARTESIAN_POINT ( 'NONE',  ( 8.329772390959197637, 2.373743296044066309, 6.857782953271941950E-17 ) ) ;
#7295 = CARTESIAN_POINT ( 'NONE',  ( 3.000000000000000888, 4.240409074144097623, 22.15038895030650679 ) ) ;
#7296 = FACE_OUTER_BOUND ( 'NONE', #3118, .T. ) ;
#7297 = ORIENTED_EDGE ( 'NONE', *, *, #3011, .F. ) ;
#7298 = AXIS2_PLACEMENT_3D ( 'NONE', #9754, #1495, #3332 ) ;
#7299 = ORIENTED_EDGE ( 'NONE', *, *, #4197, .T. ) ;
#7300 = CARTESIAN_POINT ( 'NONE',  ( -6.423942855642368777, 13.01866063961585951, 10.00000000000000000 ) ) ;
#7301 = DIRECTION ( 'NONE',  ( 1.000000000000000000, 0.000000000000000000, 0.000000000000000000 ) ) ;
#7302 = DIRECTION ( 'NONE',  ( -1.000000000000000000, 0.000000000000000000, 0.000000000000000000 ) ) ;
#7303 = AXIS2_PLACEMENT_3D ( 'NONE', #9325, #11228, #2098 ) ;
#7304 = CARTESIAN_POINT ( 'NONE',  ( 0.000000000000000000, -11.02759168516730703, -22.21333432029575050 ) ) ;
#7305 = CARTESIAN_POINT ( 'NONE',  ( -4.500000000000000888, 3.903127820947816751E-15, 3.000000000000000000 ) ) ;
#7306 = ORIENTED_EDGE ( 'NONE', *, *, #8179, .F. ) ;
#7307 = EDGE_CURVE ( 'NONE', #4079, #3976, #10880, .T. ) ;
#7308 = CARTESIAN_POINT ( 'NONE',  ( 3.000000000000000888, 0.000000000000000000, 0.000000000000000000 ) ) ;
#7309 = ORIENTED_EDGE ( 'NONE', *, *, #2477, .T. ) ;
#7310 = EDGE_CURVE ( 'NONE', #10316, #10278, #509, .T. ) ;
#7311 = EDGE_CURVE ( 'NONE', #11877, #8696, #10703, .T. ) ;
#7312 = ADVANCED_BREP_SHAPE_REPRESENTATION ( '', ( #4621, #8474 ), #10565 ) ;
#7313 = ORIENTED_EDGE ( 'NONE', *, *, #11448, .F. ) ;
#7314 = DIRECTION ( 'NONE',  ( -1.000000000000000000, -0.000000000000000000, -0.000000000000000000 ) ) ;
#7315 = DIRECTION ( 'NONE',  ( -1.000000000000000000, -0.000000000000000000, 0.000000000000000000 ) ) ;
#7316 = DIRECTION ( 'NONE',  ( -1.000000000000000000, -0.000000000000000000, 0.000000000000000000 ) ) ;
#7317 = UNCERTAINTY_MEASURE_WITH_UNIT (LENGTH_MEASURE( 1.000000000000000082E-05 ), #9205, 'distance_accuracy_value', 'NONE');
#7318 = DIRECTION ( 'NONE',  ( 1.000000000000000000, 0.000000000000000000, 0.000000000000000000 ) ) ;
#7319 = FACE_OUTER_BOUND ( 'NONE', #4787, .T. ) ;
#7320 = DIRECTION ( 'NONE',  ( -1.000000000000000000, -0.000000000000000000, 0.000000000000000000 ) ) ;
#7321 = CARTESIAN_POINT ( 'NONE',  ( 5.508953106497944674, 1.454581011951804559, 6.857782953271941950E-17 ) ) ;
#7322 = EDGE_CURVE ( 'NONE', #8746, #8808, #11567, .T. ) ;
#7323 = AXIS2_PLACEMENT_3D ( 'NONE', #9931, #3633, #7349 ) ;
#7324 = ADVANCED_FACE ( 'NONE', ( #2260 ), #5996, .T. ) ;
#7325 = CARTESIAN_POINT ( 'NONE',  ( 3.000000000000000888, 20.93895013827600593, -13.28910708463105905 ) ) ;
#7326 = ORIENTED_EDGE ( 'NONE', *, *, #11956, .T. ) ;
#7327 = ORIENTED_EDGE ( 'NONE', *, *, #4802, .T. ) ;
#7328 = DIRECTION ( 'NONE',  ( -1.000000000000000000, -0.000000000000000000, -0.000000000000000000 ) ) ;
#7329 = EDGE_LOOP ( 'NONE', ( #5249, #7285, #10528, #10907 ) ) ;
#7330 = EDGE_LOOP ( 'NONE', ( #9494, #8271, #2850, #9367 ) ) ;
#7331 = CARTESIAN_POINT ( 'NONE',  ( -3.516813791735897254, 7.717845097288996037, 10.00000000000000000 ) ) ;
#7332 = ORIENTED_EDGE ( 'NONE', *, *, #5549, .F. ) ;
#7333 = EDGE_CURVE ( 'NONE', #2104, #348, #10588, .T. ) ;
#7334 = CYLINDRICAL_SURFACE ( 'NONE', #8528, 9.599999999999997868 ) ;
#7335 = AXIS2_PLACEMENT_3D ( 'NONE', #3758, #2897, #1974 ) ;
#7336 = ORIENTED_EDGE ( 'NONE', *, *, #6545, .F. ) ;
#7337 = CARTESIAN_POINT ( 'NONE',  ( 3.000000000000000888, 20.08719549084865008, 11.20082935824082249 ) ) ;
#7338 = DIRECTION ( 'NONE',  ( 0.000000000000000000, 1.000000000000000000, 3.614007241618348376E-15 ) ) ;
#7339 = CARTESIAN_POINT ( 'NONE',  ( -5.924299593718521884, 3.297400215539481039, 10.00000000000000000 ) ) ;
#7340 = EDGE_CURVE ( 'NONE', #5268, #8050, #10484, .T. ) ;
#7341 = EDGE_CURVE ( 'NONE', #1233, #9863, #238, .T. ) ;
#7342 = DIRECTION ( 'NONE',  ( -1.000000000000000000, 0.000000000000000000, 0.000000000000000000 ) ) ;
#7343 = DIRECTION ( 'NONE',  ( -1.000000000000000000, 0.000000000000000000, 0.000000000000000000 ) ) ;
#7344 = CIRCLE ( 'NONE', #4036, 9.599999999999996092 ) ;
#7345 = ORIENTED_EDGE ( 'NONE', *, *, #7310, .T. ) ;
#7346 = CARTESIAN_POINT ( 'NONE',  ( 3.000000000000000888, 2.745295967526300451, -22.83456483164686546 ) ) ;
#7347 = ORIENTED_EDGE ( 'NONE', *, *, #5241, .T. ) ;
#7348 = CARTESIAN_POINT ( 'NONE',  ( 6.563569809674826061, -3.208372544468511833, 3.747395293195558847E-16 ) ) ;
#7349 = DIRECTION ( 'NONE',  ( 0.000000000000000000, 0.000000000000000000, 1.000000000000000000 ) ) ;
#7350 = FILL_AREA_STYLE_COLOUR ( '', #3188 ) ;
#7351 = ORIENTED_EDGE ( 'NONE', *, *, #2125, .F. ) ;
#7352 = DIRECTION ( 'NONE',  ( -1.000000000000000000, -0.000000000000000000, -0.000000000000000000 ) ) ;
#7353 = FACE_OUTER_BOUND ( 'NONE', #4063, .T. ) ;
#7354 = DIRECTION ( 'NONE',  ( -1.000000000000000000, 0.000000000000000000, 0.000000000000000000 ) ) ;
#7355 = CARTESIAN_POINT ( 'NONE',  ( 13.67726327739690184, -10.50289975150004018, 10.00000000000000000 ) ) ;
#7356 = EDGE_CURVE ( 'NONE', #6096, #5168, #2474, .T. ) ;
#7357 = CARTESIAN_POINT ( 'NONE',  ( 7.605204090343169909, 4.385345779697310320, 6.857782953271941950E-17 ) ) ;
#7358 = CARTESIAN_POINT ( 'NONE',  ( 3.000000000000000888, 18.51065745848395849, -12.88318129270159673 ) ) ;
#7359 = DIRECTION ( 'NONE',  ( 0.000000000000000000, -0.9945218953682724017, -0.1045284632676636294 ) ) ;
#7360 = ORIENTED_EDGE ( 'NONE', *, *, #7498, .T. ) ;
#7361 = CIRCLE ( 'NONE', #336, 24.80000000000000071 ) ;
#7362 = EDGE_CURVE ( 'NONE', #9796, #5920, #1695, .T. ) ;
#7363 = ORIENTED_EDGE ( 'NONE', *, *, #10970, .T. ) ;
#7364 = DIRECTION ( 'NONE',  ( -0.000000000000000000, -0.000000000000000000, -1.000000000000000000 ) ) ;
#7365 = CARTESIAN_POINT ( 'NONE',  ( -2.196651480121881050, 8.111327970581173830, 10.00000000000000000 ) ) ;
#7366 = CARTESIAN_POINT ( 'NONE',  ( 3.000000000000000888, -1.556492618230475022, -24.75110766671653906 ) ) ;
#7367 = DIRECTION ( 'NONE',  ( 0.000000000000000000, 0.000000000000000000, 1.000000000000000000 ) ) ;
#7368 = CARTESIAN_POINT ( 'NONE',  ( -8.834572391846261752, 1.442725564903823532, 3.747395293195558847E-16 ) ) ;
#7369 = CIRCLE ( 'NONE', #8364, 9.599999999999999645 ) ;
#7370 = CARTESIAN_POINT ( 'NONE',  ( 3.000000000000000888, -2.745295967526151237, 22.83456483164687967 ) ) ;
#7371 = AXIS2_PLACEMENT_3D ( 'NONE', #5722, #129, #3761 ) ;
#7372 = CARTESIAN_POINT ( 'NONE',  ( 3.000000000000000888, -22.42251312757876036, -5.117118920208720390 ) ) ;
#7373 = EDGE_LOOP ( 'NONE', ( #2851, #165, #11397, #2014 ) ) ;
#7374 = ORIENTED_EDGE ( 'NONE', *, *, #338, .F. ) ;
#7375 = ORIENTED_EDGE ( 'NONE', *, *, #3888, .T. ) ;
#7376 = DIRECTION ( 'NONE',  ( 0.000000000000000000, 0.000000000000000000, 1.000000000000000000 ) ) ;
#7377 = CARTESIAN_POINT ( 'NONE',  ( 3.000000000000000888, -22.83456483164690809, 2.745295967525920311 ) ) ;
#7378 =( REPRESENTATION_RELATIONSHIP ('NONE','NONE', #8743, #6698 ) REPRESENTATION_RELATIONSHIP_WITH_TRANSFORMATION ( #6046 )SHAPE_REPRESENTATION_RELATIONSHIP( ) );
#7379 = CIRCLE ( 'NONE', #1333, 9.599999999999997868 ) ;
#7380 = DIRECTION ( 'NONE',  ( -1.000000000000000000, 0.000000000000000000, -0.000000000000000000 ) ) ;
#7381 = CARTESIAN_POINT ( 'NONE',  ( 3.000000000000000888, 0.000000000000000000, 0.000000000000000000 ) ) ;
#7382 = ADVANCED_FACE ( 'NONE', ( #10081 ), #4336, .T. ) ;
#7383 = CARTESIAN_POINT ( 'NONE',  ( -8.207979594962566239, -13.19054478262514252, 3.747395293195558847E-16 ) ) ;
#7384 = CARTESIAN_POINT ( 'NONE',  ( 1.018538006779708738, -7.771884277300779686, 6.857782953271941950E-17 ) ) ;
#7385 = DIRECTION ( 'NONE',  ( -1.000000000000000000, 0.000000000000000000, 0.000000000000000000 ) ) ;
#7386 = CIRCLE ( 'NONE', #2323, 22.99899999999999878 ) ;
#7387 = EDGE_CURVE ( 'NONE', #7388, #5574, #1585, .T. ) ;
#7388 = VERTEX_POINT ( 'NONE', #10889 ) ;
#7389 = ORIENTED_EDGE ( 'NONE', *, *, #4728, .F. ) ;
#7390 = MECHANICAL_DESIGN_GEOMETRIC_PRESENTATION_REPRESENTATION (  '', ( #9152 ), #8771 ) ;
#7391 = CARTESIAN_POINT ( 'NONE',  ( 0.000000000000000000, 0.4575788569254873317, -22.54798042742717712 ) ) ;
#7392 = ORIENTED_EDGE ( 'NONE', *, *, #2175, .T. ) ;
#7393 = VERTEX_POINT ( 'NONE', #8933 ) ;
#7394 = CARTESIAN_POINT ( 'NONE',  ( -5.920784292471868326, 6.290491683487167585, 10.00000000000000000 ) ) ;
#7395 = EDGE_CURVE ( 'NONE', #4467, #4143, #6303, .T. ) ;
#7396 = ORIENTED_EDGE ( 'NONE', *, *, #6404, .F. ) ;
#7397 = DIRECTION ( 'NONE',  ( -1.000000000000000000, 0.000000000000000000, -0.000000000000000000 ) ) ;
#7398 = ORIENTED_EDGE ( 'NONE', *, *, #4810, .T. ) ;
#7399 = EDGE_CURVE ( 'NONE', #2310, #9213, #11065, .T. ) ;
#7400 = CIRCLE ( 'NONE', #2127, 9.599999999999997868 ) ;
#7401 = CARTESIAN_POINT ( 'NONE',  ( 0.000000000000000000, -18.80635025205160815, -13.23915371906974592 ) ) ;
#7402 = ADVANCED_FACE ( 'NONE', ( #781 ), #9110, .T. ) ;
#7403 = DIRECTION ( 'NONE',  ( 0.000000000000000000, -6.982962677686266711E-15, 1.000000000000000000 ) ) ;
#7404 = CARTESIAN_POINT ( 'NONE',  ( 5.267519402444160725, 2.381954139586888175, 10.00000000000000000 ) ) ;
#7405 = DIRECTION ( 'NONE',  ( -1.000000000000000000, 0.000000000000000000, 0.000000000000000000 ) ) ;
#7406 = CARTESIAN_POINT ( 'NONE',  ( 3.000000000000000888, -6.168200451485582825, -24.02068490260619171 ) ) ;
#7407 = ORIENTED_EDGE ( 'NONE', *, *, #893, .F. ) ;
#7408 = ORIENTED_EDGE ( 'NONE', *, *, #6988, .F. ) ;
#7409 = LINE ( 'NONE', #8471, #400 ) ;
#7410 = EDGE_LOOP ( 'NONE', ( #9907, #1442, #5390, #1293 ) ) ;
#7411 = AXIS2_PLACEMENT_3D ( 'NONE', #6412, #4454, #5381 ) ;
#7412 = CIRCLE ( 'NONE', #3125, 22.99899999999999523 ) ;
#7413 = CARTESIAN_POINT ( 'NONE',  ( -5.319913005755192437, -3.351504787100450855, 3.747395293195558847E-16 ) ) ;
#7414 = VECTOR ( 'NONE', #5490, 1000.000000000000000 ) ;
#7415 = CARTESIAN_POINT ( 'NONE',  ( 3.000000000000000888, -22.21333432029556221, -11.02759168516767474 ) ) ;
#7416 = CARTESIAN_POINT ( 'NONE',  ( 3.000000000000000888, 22.54798042742717712, 0.4575788569255671012 ) ) ;
#7417 = DIRECTION ( 'NONE',  ( 0.000000000000000000, -0.5877852522924797984, 0.8090169943749425663 ) ) ;
#7418 = DIRECTION ( 'NONE',  ( 1.000000000000000000, 0.000000000000000000, 0.000000000000000000 ) ) ;
#7419 = CARTESIAN_POINT ( 'NONE',  ( -6.825012239887737309, 1.243808647927286515, 6.857782953271941950E-17 ) ) ;
#7420 = DIRECTION ( 'NONE',  ( 0.000000000000000000, 0.000000000000000000, 1.000000000000000000 ) ) ;
#7421 = CIRCLE ( 'NONE', #3909, 9.599999999999999645 ) ;
#7422 = DIRECTION ( 'NONE',  ( 0.000000000000000000, -0.6691306063588494668, -0.7431448254774020157 ) ) ;
#7423 = ORIENTED_EDGE ( 'NONE', *, *, #5832, .F. ) ;
#7424 = VERTEX_POINT ( 'NONE', #7077 ) ;
#7425 = AXIS2_PLACEMENT_3D ( 'NONE', #8952, #2402, #4296 ) ;
#7426 = EDGE_CURVE ( 'NONE', #8709, #7274, #2680, .T. ) ;
#7427 = DIRECTION ( 'NONE',  ( -1.000000000000000000, -0.000000000000000000, -0.000000000000000000 ) ) ;
#7428 = AXIS2_PLACEMENT_3D ( 'NONE', #9063, #672, #10772 ) ;
#7429 = CARTESIAN_POINT ( 'NONE',  ( -8.834572391846261752, 1.442725564903824420, 10.00000000000000000 ) ) ;
#7430 = VECTOR ( 'NONE', #4736, 1000.000000000000000 ) ;
#7431 = DIRECTION ( 'NONE',  ( 0.000000000000000000, 0.000000000000000000, 1.000000000000000000 ) ) ;
#7432 = FACE_OUTER_BOUND ( 'NONE', #8889, .T. ) ;
#7433 = CARTESIAN_POINT ( 'NONE',  ( -3.141381368648054284, 10.98006565327106188, 3.747395293195558847E-16 ) ) ;
#7434 = EDGE_CURVE ( 'NONE', #6148, #3183, #10685, .T. ) ;
#7435 = CARTESIAN_POINT ( 'NONE',  ( 3.194803811556592876, -2.743189786380903161, 3.747395293195558847E-16 ) ) ;
#7436 = AXIS2_PLACEMENT_3D ( 'NONE', #1720, #8211, #7469 ) ;
#7437 = DIRECTION ( 'NONE',  ( -1.000000000000000000, -0.000000000000000000, -0.000000000000000000 ) ) ;
#7438 = VECTOR ( 'NONE', #7561, 1000.000000000000000 ) ;
#7439 = CIRCLE ( 'NONE', #4315, 22.99899999999999878 ) ;
#7440 = VERTEX_POINT ( 'NONE', #3609 ) ;
#7441 = ORIENTED_EDGE ( 'NONE', *, *, #3070, .F. ) ;
#7442 = ORIENTED_EDGE ( 'NONE', *, *, #2275, .F. ) ;
#7443 = DIRECTION ( 'NONE',  ( 0.000000000000000000, 0.000000000000000000, 1.000000000000000000 ) ) ;
#7444 = LINE ( 'NONE', #8503, #6665 ) ;
#7445 = CIRCLE ( 'NONE', #6471, 22.99899999999999878 ) ;
#7446 = AXIS2_PLACEMENT_3D ( 'NONE', #5472, #6570, #5540 ) ;
#7447 = CARTESIAN_POINT ( 'NONE',  ( 3.000000000000000888, 21.30300407174362576, -7.402892494506364329 ) ) ;
#7448 = DIRECTION ( 'NONE',  ( 0.000000000000000000, 0.000000000000000000, 1.000000000000000000 ) ) ;
#7449 = VECTOR ( 'NONE', #1199, 1000.000000000000000 ) ;
#7450 = AXIS2_PLACEMENT_3D ( 'NONE', #1209, #2361, #7691 ) ;
#7451 = LINE ( 'NONE', #2814, #2410 ) ;
#7452 = CARTESIAN_POINT ( 'NONE',  ( 11.04976219204102783, -11.79656285006036676, 3.747395293195558847E-16 ) ) ;
#7453 = CARTESIAN_POINT ( 'NONE',  ( 8.527474615971319949, 0.9793716136081375145, 6.857782953271941950E-17 ) ) ;
#7454 = DIRECTION ( 'NONE',  ( -1.000000000000000000, 0.000000000000000000, 0.000000000000000000 ) ) ;
#7455 = ORIENTED_EDGE ( 'NONE', *, *, #10084, .F. ) ;
#7456 = ORIENTED_EDGE ( 'NONE', *, *, #9094, .T. ) ;
#7457 = CARTESIAN_POINT ( 'NONE',  ( -10.00000000000000000, 0.000000000000000000, 0.000000000000000000 ) ) ;
#7458 = CIRCLE ( 'NONE', #8814, 24.80000000000000071 ) ;
#7459 = ORIENTED_EDGE ( 'NONE', *, *, #7900, .T. ) ;
#7460 = ORIENTED_EDGE ( 'NONE', *, *, #3223, .F. ) ;
#7461 = DIRECTION ( 'NONE',  ( -1.000000000000000000, 0.000000000000000000, 0.000000000000000000 ) ) ;
#7462 = DIRECTION ( 'NONE',  ( -0.000000000000000000, -0.000000000000000000, -1.000000000000000000 ) ) ;
#7463 = EDGE_LOOP ( 'NONE', ( #367, #5100, #11302, #3036 ) ) ;
#7464 = AXIS2_PLACEMENT_3D ( 'NONE', #5325, #11983, #3549 ) ;
#7465 = DIRECTION ( 'NONE',  ( 1.000000000000000000, 0.000000000000000000, 0.000000000000000000 ) ) ;
#7466 = DIRECTION ( 'NONE',  ( -1.000000000000000000, 0.000000000000000000, -0.000000000000000000 ) ) ;
#7467 = CARTESIAN_POINT ( 'NONE',  ( -7.575117642440518217, -14.74712341115846392, 6.857782953271941950E-17 ) ) ;
#7468 = FACE_OUTER_BOUND ( 'NONE', #8882, .T. ) ;
#7469 = DIRECTION ( 'NONE',  ( 0.000000000000000000, -6.866613759074863256E-15, 1.000000000000000000 ) ) ;
#7470 = ORIENTED_EDGE ( 'NONE', *, *, #10394, .T. ) ;
#7471 = ORIENTED_EDGE ( 'NONE', *, *, #6149, .F. ) ;
#7472 = CARTESIAN_POINT ( 'NONE',  ( 3.000000000000000888, -22.99643626497957172, 0.3433949777330864706 ) ) ;
#7473 = ADVANCED_FACE ( 'NONE', ( #10023 ), #4397, .T. ) ;
#7474 = ORIENTED_EDGE ( 'NONE', *, *, #12045, .F. ) ;
#7475 = MECHANICAL_DESIGN_GEOMETRIC_PRESENTATION_REPRESENTATION (  '', ( #6110 ), #1811 ) ;
#7476 = ADVANCED_FACE ( 'NONE', ( #4275 ), #9962, .T. ) ;
#7477 = CARTESIAN_POINT ( 'NONE',  ( 6.600721363681033793, -14.58171973507987751, 10.00000000000000000 ) ) ;
#7478 = PRESENTATION_LAYER_ASSIGNMENT (  '', '', ( #11594 ) ) ;
#7479 = LINE ( 'NONE', #10239, #3451 ) ;
#7480 =( NAMED_UNIT ( * ) PLANE_ANGLE_UNIT ( ) SI_UNIT ( $, .RADIAN. ) );
#7481 = ORIENTED_EDGE ( 'NONE', *, *, #6213, .F. ) ;
#7482 = DIRECTION ( 'NONE',  ( 0.000000000000000000, -0.6691306063588495778, -0.7431448254774020157 ) ) ;
#7483 = CARTESIAN_POINT ( 'NONE',  ( 0.000000000000000000, 24.53384959170457336, 3.623565124517186931 ) ) ;
#7484 = CARTESIAN_POINT ( 'NONE',  ( -15.85416723795449556, 2.087521067385502693, 10.00000000000000000 ) ) ;
#7485 = AXIS2_PLACEMENT_3D ( 'NONE', #9310, #2760, #5635 ) ;
#7486 = CARTESIAN_POINT ( 'NONE',  ( -4.263796145714473518, -6.152586724582786104, 6.857782953271941950E-17 ) ) ;
#7487 =( NAMED_UNIT ( * ) PLANE_ANGLE_UNIT ( ) SI_UNIT ( $, .RADIAN. ) );
#7488 = ADVANCED_FACE ( 'NONE', ( #11856 ), #3431, .T. ) ;
#7489 = FACE_OUTER_BOUND ( 'NONE', #3482, .T. ) ;
#7490 = AXIS2_PLACEMENT_3D ( 'NONE', #8372, #6469, #10206 ) ;
#7491 = VECTOR ( 'NONE', #2377, 1000.000000000000000 ) ;
#7492 = ORIENTED_EDGE ( 'NONE', *, *, #7341, .F. ) ;
#7493 = ORIENTED_EDGE ( 'NONE', *, *, #3890, .F. ) ;
#7494 = EDGE_LOOP ( 'NONE', ( #1455, #4718, #10389, #7829 ) ) ;
#7495 = CARTESIAN_POINT ( 'NONE',  ( 3.000000000000000888, 19.43515443678402832, 15.40502424595151254 ) ) ;
#7496 = CARTESIAN_POINT ( 'NONE',  ( -8.109405675831295568, 8.372220220303479010, 10.00000000000000000 ) ) ;
#7497 = DIRECTION ( 'NONE',  ( 0.000000000000000000, -0.7431448254773999063, 0.6691306063588519093 ) ) ;
#7498 = EDGE_CURVE ( 'NONE', #9819, #8966, #7258, .T. ) ;
#7499 = CARTESIAN_POINT ( 'NONE',  ( 9.701579622837702033, -3.641351606116561612, 3.747395293195558847E-16 ) ) ;
#7500 = CARTESIAN_POINT ( 'NONE',  ( 3.000000000000000888, 0.000000000000000000, 0.000000000000000000 ) ) ;
#7501 = ADVANCED_FACE ( 'NONE', ( #539 ), #603, .T. ) ;
#7502 = AXIS2_PLACEMENT_3D ( 'NONE', #8107, #5535, #4618 ) ;
#7503 = DIRECTION ( 'NONE',  ( 1.000000000000000000, -0.000000000000000000, -0.000000000000000000 ) ) ;
#7504 = ORIENTED_EDGE ( 'NONE', *, *, #3077, .T. ) ;
#7505 = ORIENTED_EDGE ( 'NONE', *, *, #6805, .T. ) ;
#7506 = ORIENTED_EDGE ( 'NONE', *, *, #170, .F. ) ;
#7507 = ORIENTED_EDGE ( 'NONE', *, *, #11815, .T. ) ;
#7508 = CARTESIAN_POINT ( 'NONE',  ( 3.000000000000000888, 18.80635025205169697, 13.23915371906961447 ) ) ;
#7509 = CARTESIAN_POINT ( 'NONE',  ( 3.000000000000000888, 2.811977935937781670, 22.37663021667345120 ) ) ;
#7510 = ADVANCED_FACE ( 'NONE', ( #6238 ), #3488, .T. ) ;
#7511 = AXIS2_PLACEMENT_3D ( 'NONE', #11518, #9807, #6139 ) ;
#7512 = CARTESIAN_POINT ( 'NONE',  ( 0.000000000000000000, 0.000000000000000000, 1.000000000000000000 ) ) ;
#7513 = DIRECTION ( 'NONE',  ( 0.000000000000000000, 0.000000000000000000, 1.000000000000000000 ) ) ;
#7514 = FACE_OUTER_BOUND ( 'NONE', #704, .T. ) ;
#7515 = CARTESIAN_POINT ( 'NONE',  ( 2.839002905303027013, -15.63284973865750693, 3.747395293195558847E-16 ) ) ;
#7516 = CARTESIAN_POINT ( 'NONE',  ( 3.000000000000000888, 0.000000000000000000, 0.000000000000000000 ) ) ;
#7517 = FACE_OUTER_BOUND ( 'NONE', #6941, .T. ) ;
#7518 = VERTEX_POINT ( 'NONE', #12039 ) ;
#7519 = ORIENTED_EDGE ( 'NONE', *, *, #1207, .T. ) ;
#7520 = CARTESIAN_POINT ( 'NONE',  ( 3.000000000000000888, -17.71842311621518107, -17.35216073792458502 ) ) ;
#7521 = ORIENTED_EDGE ( 'NONE', *, *, #1369, .F. ) ;
#7522 = EDGE_CURVE ( 'NONE', #2524, #1721, #7184, .T. ) ;
#7523 = CARTESIAN_POINT ( 'NONE',  ( 4.525508228541173850, -0.2388087992699347017, 10.00000000000000000 ) ) ;
#7524 = ADVANCED_FACE ( 'NONE', ( #5501 ), #1758, .T. ) ;
#7525 = DIRECTION ( 'NONE',  ( -1.000000000000000000, 0.000000000000000000, 0.000000000000000000 ) ) ;
#7526 = ORIENTED_EDGE ( 'NONE', *, *, #2305, .F. ) ;
#7527 = CARTESIAN_POINT ( 'NONE',  ( 3.000000000000000888, 21.97702544527757951, 6.779701584702809924 ) ) ;
#7528 = DIRECTION ( 'NONE',  ( -1.000000000000000000, -0.000000000000000000, -0.000000000000000000 ) ) ;
#7529 = CARTESIAN_POINT ( 'NONE',  ( 5.312937634500610073, -1.259815497212794400, 10.00000000000000000 ) ) ;
#7530 = CARTESIAN_POINT ( 'NONE',  ( 3.000000000000000888, -1.039229259764660407, 24.77821629063821263 ) ) ;
#7531 = CARTESIAN_POINT ( 'NONE',  ( 3.000000000000000888, -2.062268319295407881, -22.90635393027948297 ) ) ;
#7532 = LINE ( 'NONE', #11276, #5506 ) ;
#7533 = ORIENTED_EDGE ( 'NONE', *, *, #709, .F. ) ;
#7534 = ORIENTED_EDGE ( 'NONE', *, *, #2324, .T. ) ;
#7535 = DIRECTION ( 'NONE',  ( -1.000000000000000000, -0.000000000000000000, -0.000000000000000000 ) ) ;
#7536 = ORIENTED_EDGE ( 'NONE', *, *, #9202, .F. ) ;
#7537 = AXIS2_PLACEMENT_3D ( 'NONE', #10419, #3936, #6742 ) ;
#7538 = CARTESIAN_POINT ( 'NONE',  ( -12.61273389267918610, -8.731886703670456384, 10.00000000000000000 ) ) ;
#7539 = CARTESIAN_POINT ( 'NONE',  ( 3.000000000000000888, 18.51065745848377730, 12.88318129270185430 ) ) ;
#7540 = CARTESIAN_POINT ( 'NONE',  ( 3.000000000000000888, -13.79477846460808799, 18.40266524480583854 ) ) ;
#7541 = DIRECTION ( 'NONE',  ( 0.000000000000000000, -0.8090169943749407899, -0.5877852522924822409 ) ) ;
#7542 = CARTESIAN_POINT ( 'NONE',  ( -1.999398781552333970, 15.23274265415849626, 10.00000000000000000 ) ) ;
#7543 = DIRECTION ( 'NONE',  ( 0.000000000000000000, 0.000000000000000000, 1.000000000000000000 ) ) ;
#7544 = DIRECTION ( 'NONE',  ( -1.000000000000000000, -0.000000000000000000, -0.000000000000000000 ) ) ;
#7545 = ADVANCED_FACE ( 'NONE', ( #4768 ), #11310, .T. ) ;
#7546 = DIRECTION ( 'NONE',  ( 1.000000000000000000, 0.000000000000000000, 0.000000000000000000 ) ) ;
#7547 = CARTESIAN_POINT ( 'NONE',  ( 3.000000000000000888, -22.15038895030646060, -4.240409074144325885 ) ) ;
#7548 = EDGE_LOOP ( 'NONE', ( #9469, #11865, #11973, #10133 ) ) ;
#7549 = DIRECTION ( 'NONE',  ( 0.000000000000000000, 0.000000000000000000, 1.000000000000000000 ) ) ;
#7550 = PRODUCT_DEFINITION_SHAPE ( 'NONE', 'NONE',  #12119 ) ;
#7551 = ORIENTED_EDGE ( 'NONE', *, *, #1247, .F. ) ;
#7552 = VECTOR ( 'NONE', #11801, 1000.000000000000000 ) ;
#7553 = FACE_OUTER_BOUND ( 'NONE', #11361, .T. ) ;
#7554 = CARTESIAN_POINT ( 'NONE',  ( -5.773631947676831189, 9.989728373610905265, 10.00000000000000000 ) ) ;
#7555 = SHAPE_REPRESENTATION ( 'spring', ( #8474 ), #10565 ) ;
#7556 = ADVANCED_FACE ( 'NONE', ( #11124 ), #5620, .F. ) ;
#7557 = CARTESIAN_POINT ( 'NONE',  ( 3.000000000000000888, 0.000000000000000000, 0.000000000000000000 ) ) ;
#7558 = EDGE_CURVE ( 'NONE', #6311, #9956, #2742, .T. ) ;
#7559 = CARTESIAN_POINT ( 'NONE',  ( -5.359287035703753865, 6.724520318540387009, 3.747395293195558847E-16 ) ) ;
#7560 = CARTESIAN_POINT ( 'NONE',  ( 0.5697670706242773386, -3.781298318517893442, 3.747395293195558847E-16 ) ) ;
#7561 = DIRECTION ( 'NONE',  ( 1.000000000000000000, -0.000000000000000000, 0.000000000000000000 ) ) ;
#7562 = ORIENTED_EDGE ( 'NONE', *, *, #3965, .T. ) ;
#7563 = ORIENTED_EDGE ( 'NONE', *, *, #3756, .F. ) ;
#7564 = ORIENTED_EDGE ( 'NONE', *, *, #8904, .F. ) ;
#7565 = FACE_OUTER_BOUND ( 'NONE', #1113, .T. ) ;
#7566 = DIRECTION ( 'NONE',  ( 0.000000000000000000, 0.8660254037844363761, 0.5000000000000039968 ) ) ;
#7567 = CARTESIAN_POINT ( 'NONE',  ( 3.000000000000000888, -22.37663021667341923, 6.788022064061986605 ) ) ;
#7568 = DIRECTION ( 'NONE',  ( 0.000000000000000000, 0.000000000000000000, 1.000000000000000000 ) ) ;
#7569 = AXIS2_PLACEMENT_3D ( 'NONE', #8958, #11535, #4134 ) ;
#7570 = DIRECTION ( 'NONE',  ( -1.000000000000000000, -0.000000000000000000, 0.000000000000000000 ) ) ;
#7571 = CARTESIAN_POINT ( 'NONE',  ( 13.29800827116429573, 3.099979537169514909, 3.747395293195558847E-16 ) ) ;
#7572 = DIRECTION ( 'NONE',  ( -1.000000000000000000, 0.000000000000000000, 0.000000000000000000 ) ) ;
#7573 = VERTEX_POINT ( 'NONE', #10142 ) ;
#7574 = ORIENTED_EDGE ( 'NONE', *, *, #5184, .T. ) ;
#7575 = CARTESIAN_POINT ( 'NONE',  ( -8.739072045530903665, -14.04184524613901353, 10.00000000000000000 ) ) ;
#7576 = ORIENTED_EDGE ( 'NONE', *, *, #10921, .T. ) ;
#7577 = CIRCLE ( 'NONE', #3092, 9.599999999999997868 ) ;
#7578 = CARTESIAN_POINT ( 'NONE',  ( 1.500000000000000444, 15.80756504416690866, 19.10918332567963773 ) ) ;
#7579 = ADVANCED_FACE ( 'NONE', ( #4587 ), #8376, .T. ) ;
#7580 = DIRECTION ( 'NONE',  ( -0.000000000000000000, -0.000000000000000000, 1.000000000000000000 ) ) ;
#7581 = ORIENTED_EDGE ( 'NONE', *, *, #5239, .F. ) ;
#7582 = DIRECTION ( 'NONE',  ( -0.000000000000000000, -0.000000000000000000, 1.000000000000000000 ) ) ;
#7583 = DIRECTION ( 'NONE',  ( 1.000000000000000000, 0.000000000000000000, 0.000000000000000000 ) ) ;
#7584 = CARTESIAN_POINT ( 'NONE',  ( -13.04979933117209256, -0.2127334381860506995, 6.857782953271941950E-17 ) ) ;
#7585 = AXIS2_PLACEMENT_3D ( 'NONE', #8506, #3848, #7813 ) ;
#7586 = VECTOR ( 'NONE', #3109, 1000.000000000000000 ) ;
#7587 = DIRECTION ( 'NONE',  ( -1.000000000000000000, 0.000000000000000000, 0.000000000000000000 ) ) ;
#7588 = EDGE_CURVE ( 'NONE', #4018, #6189, #44, .T. ) ;
#7589 = DIRECTION ( 'NONE',  ( 0.000000000000000000, 0.000000000000000000, 1.000000000000000000 ) ) ;
#7590 = ORIENTED_EDGE ( 'NONE', *, *, #626, .T. ) ;
#7591 = ORIENTED_EDGE ( 'NONE', *, *, #2922, .F. ) ;
#7592 = DIRECTION ( 'NONE',  ( 0.000000000000000000, 0.000000000000000000, -1.000000000000000000 ) ) ;
#7593 = ORIENTED_EDGE ( 'NONE', *, *, #2465, .T. ) ;
#7594 = CARTESIAN_POINT ( 'NONE',  ( 3.885483365683945145, 13.62125166200965332, 10.00000000000000000 ) ) ;
#7595 = CIRCLE ( 'NONE', #5251, 9.599999999999996092 ) ;
#7596 = CARTESIAN_POINT ( 'NONE',  ( 3.000000000000000888, -23.88662356770119644, 6.668524164681547184 ) ) ;
#7597 = CARTESIAN_POINT ( 'NONE',  ( 3.000000000000000888, 11.48910920600714647, -21.97817939804027532 ) ) ;
#7598 = DIRECTION ( 'NONE',  ( 0.000000000000000000, 0.000000000000000000, 1.000000000000000000 ) ) ;
#7599 = CARTESIAN_POINT ( 'NONE',  ( 9.623984404418655103, 6.889883918979096578, 10.00000000000000000 ) ) ;
#7600 = SURFACE_SIDE_STYLE ('',( #6688 ) ) ;
#7601 = DIRECTION ( 'NONE',  ( 0.000000000000000000, 0.000000000000000000, 1.000000000000000000 ) ) ;
#7602 = AXIS2_PLACEMENT_3D ( 'NONE', #5194, #7427, #536 ) ;
#7603 = DIRECTION ( 'NONE',  ( 1.000000000000000000, 0.000000000000000000, 0.000000000000000000 ) ) ;
#7604 = ORIENTED_EDGE ( 'NONE', *, *, #7005, .T. ) ;
#7605 = DIRECTION ( 'NONE',  ( 1.000000000000000000, 0.000000000000000000, -0.000000000000000000 ) ) ;
#7606 = CIRCLE ( 'NONE', #974, 9.599999999999997868 ) ;
#7607 = EDGE_LOOP ( 'NONE', ( #36, #2372, #11206, #7138 ) ) ;
#7608 = CARTESIAN_POINT ( 'NONE',  ( 0.000000000000000000, 22.47229024614977533, 1.901833551798334909 ) ) ;
#7609 = CARTESIAN_POINT ( 'NONE',  ( -5.920784292471868326, 6.290491683487167585, 10.00000000000000000 ) ) ;
#7610 = CARTESIAN_POINT ( 'NONE',  ( 0.000000000000000000, -22.42251312757883142, 5.117118920208414856 ) ) ;
#7611 = CARTESIAN_POINT ( 'NONE',  ( 1.831757423467612389, 7.960349185506225389, 3.747395293195558847E-16 ) ) ;
#7612 = ADVANCED_FACE ( 'NONE', ( #1827 ), #10388, .T. ) ;
#7613 = CARTESIAN_POINT ( 'NONE',  ( -7.575117642440518217, -14.74712341115846392, 6.857782953271941950E-17 ) ) ;
#7614 = DIRECTION ( 'NONE',  ( -1.000000000000000000, 0.000000000000000000, 0.000000000000000000 ) ) ;
#7615 = ORIENTED_EDGE ( 'NONE', *, *, #9914, .F. ) ;
#7616 = AXIS2_PLACEMENT_3D ( 'NONE', #4682, #11103, #827 ) ;
#7617 = ADVANCED_FACE ( 'NONE', ( #3904 ), #9475, .T. ) ;
#7618 = EDGE_CURVE ( 'NONE', #2737, #9019, #12097, .T. ) ;
#7619 = CIRCLE ( 'NONE', #10171, 22.99899999999999878 ) ;
#7620 = ORIENTED_EDGE ( 'NONE', *, *, #4340, .T. ) ;
#7621 = CARTESIAN_POINT ( 'NONE',  ( 1.500000000000000444, 13.28910708463128287, 20.93895013827586382 ) ) ;
#7622 = FACE_OUTER_BOUND ( 'NONE', #8869, .T. ) ;
#7623 = ADVANCED_FACE ( 'NONE', ( #1945 ), #1091, .T. ) ;
#7624 = VERTEX_POINT ( 'NONE', #4823 ) ;
#7625 = CARTESIAN_POINT ( 'NONE',  ( 3.000000000000000888, -17.97274125076083351, 13.62355943574013750 ) ) ;
#7626 = CARTESIAN_POINT ( 'NONE',  ( 3.000000000000000888, 0.000000000000000000, 0.000000000000000000 ) ) ;
#7627 = CIRCLE ( 'NONE', #7826, 9.600000000000001421 ) ;
#7628 = DIRECTION ( 'NONE',  ( -1.000000000000000000, 0.000000000000000000, 0.000000000000000000 ) ) ;
#7629 = VECTOR ( 'NONE', #8510, 1000.000000000000000 ) ;
#7630 = CARTESIAN_POINT ( 'NONE',  ( 0.4634152073531430105, 14.27464310366533340, 3.747395293195558847E-16 ) ) ;
#7631 =( GEOMETRIC_REPRESENTATION_CONTEXT ( 3 ) GLOBAL_UNCERTAINTY_ASSIGNED_CONTEXT ( ( #8812 ) ) GLOBAL_UNIT_ASSIGNED_CONTEXT ( ( #7845, #6009, #2096 ) ) REPRESENTATION_CONTEXT ( 'NONE', 'WORKASPACE' ) );
#7632 = EDGE_CURVE ( 'NONE', #2061, #10333, #3722, .T. ) ;
#7633 = CARTESIAN_POINT ( 'NONE',  ( 3.000000000000000888, -22.54798042742718422, 0.4575788569251160731 ) ) ;
#7634 = ORIENTED_EDGE ( 'NONE', *, *, #626, .F. ) ;
#7635 = VERTEX_POINT ( 'NONE', #2991 ) ;
#7636 = DIRECTION ( 'NONE',  ( 0.000000000000000000, 0.000000000000000000, 1.000000000000000000 ) ) ;
#7637 = CARTESIAN_POINT ( 'NONE',  ( 17.50000000000000000, 0.000000000000000000, 10.00000000000000000 ) ) ;
#7638 = CIRCLE ( 'NONE', #4130, 22.99899999999999523 ) ;
#7639 = EDGE_LOOP ( 'NONE', ( #8114, #11796, #7423, #1291 ) ) ;
#7640 = VECTOR ( 'NONE', #245, 1000.000000000000000 ) ;
#7641 = LINE ( 'NONE', #3005, #61 ) ;
#7642 = AXIS2_PLACEMENT_3D ( 'NONE', #9029, #6339, #4308 ) ;
#7643 = VECTOR ( 'NONE', #4947, 1000.000000000000000 ) ;
#7644 = DIRECTION ( 'NONE',  ( 1.000000000000000000, 0.000000000000000000, -0.000000000000000000 ) ) ;
#7645 = ORIENTED_EDGE ( 'NONE', *, *, #4369, .T. ) ;
#7646 = DIRECTION ( 'NONE',  ( -1.000000000000000000, 0.000000000000000000, 0.000000000000000000 ) ) ;
#7647 = ADVANCED_FACE ( 'NONE', ( #2812, #967 ), #8446, .T. ) ;
#7648 = CARTESIAN_POINT ( 'NONE',  ( -10.00000000000000000, 0.000000000000000000, 0.000000000000000000 ) ) ;
#7649 = CARTESIAN_POINT ( 'NONE',  ( 11.14370178440675474, -8.845034901279911210, 6.857782953271941950E-17 ) ) ;
#7650 = AXIS2_PLACEMENT_3D ( 'NONE', #8400, #4668, #9336 ) ;
#7651 = CARTESIAN_POINT ( 'NONE',  ( 3.000000000000000888, -16.45023496161654819, -15.42759117534402513 ) ) ;
#7652 = ORIENTED_EDGE ( 'NONE', *, *, #9512, .F. ) ;
#7653 = VECTOR ( 'NONE', #4377, 1000.000000000000000 ) ;
#7654 = ADVANCED_FACE ( 'NONE', ( #5680 ), #1038, .T. ) ;
#7655 = PLANE ( 'NONE',  #406 ) ;
#7656 = EDGE_LOOP ( 'NONE', ( #8924, #1501, #3484, #7590 ) ) ;
#7657 = ORIENTED_EDGE ( 'NONE', *, *, #3888, .F. ) ;
#7658 = CARTESIAN_POINT ( 'NONE',  ( 0.000000000000000000, 0.000000000000000000, 20.00000000000000000 ) ) ;
#7659 = ORIENTED_EDGE ( 'NONE', *, *, #2347, .T. ) ;
#7660 = CARTESIAN_POINT ( 'NONE',  ( 7.795318149608632119, -14.02504990430958998, 10.00000000000000000 ) ) ;
#7661 = STYLED_ITEM ( 'NONE', ( #9567 ), #302 ) ;
#7662 = AXIS2_PLACEMENT_3D ( 'NONE', #6909, #10652, #2265 ) ;
#7663 = CARTESIAN_POINT ( 'NONE',  ( 0.000000000000000000, 13.72351598154924979, -20.65684170206477788 ) ) ;
#7664 = CARTESIAN_POINT ( 'NONE',  ( 17.24531215409252383, -2.853661713830123237, 6.857782953271941950E-17 ) ) ;
#7665 = ADVANCED_FACE ( 'NONE', ( #7933 ), #7752, .T. ) ;
#7666 = CARTESIAN_POINT ( 'NONE',  ( 3.000000000000000888, 0.000000000000000000, 0.000000000000000000 ) ) ;
#7667 = DIRECTION ( 'NONE',  ( -1.000000000000000000, -0.000000000000000000, -0.000000000000000000 ) ) ;
#7668 = CARTESIAN_POINT ( 'NONE',  ( 13.06601448280975220, -5.920767845834314258, 10.00000000000000000 ) ) ;
#7669 = CARTESIAN_POINT ( 'NONE',  ( 3.000000000000000888, -5.135568396239877487, -21.96011696265496838 ) ) ;
#7670 = DIRECTION ( 'NONE',  ( -1.000000000000000000, 0.000000000000000000, 0.000000000000000000 ) ) ;
#7671 = FACE_OUTER_BOUND ( 'NONE', #5113, .T. ) ;
#7672 = AXIS2_PLACEMENT_3D ( 'NONE', #1027, #9221, #2859 ) ;
#7673 = ORIENTED_EDGE ( 'NONE', *, *, #7588, .F. ) ;
#7674 = CARTESIAN_POINT ( 'NONE',  ( 3.000000000000000888, 17.71842311621552923, -17.35216073792422620 ) ) ;
#7675 = VERTEX_POINT ( 'NONE', #4885 ) ;
#7676 = VERTEX_POINT ( 'NONE', #3967 ) ;
#7677 = EDGE_CURVE ( 'NONE', #8902, #9734, #7379, .T. ) ;
#7678 = DIRECTION ( 'NONE',  ( -1.000000000000000000, 0.000000000000000000, 0.000000000000000000 ) ) ;
#7679 = CARTESIAN_POINT ( 'NONE',  ( -5.541928854458318732, -2.884958602215172974, 10.00000000000000000 ) ) ;
#7680 = CIRCLE ( 'NONE', #5929, 24.80000000000000071 ) ;
#7681 = CARTESIAN_POINT ( 'NONE',  ( 0.000000000000000000, 11.02759168516744737, 22.21333432029567589 ) ) ;
#7682 = CARTESIAN_POINT ( 'NONE',  ( 8.329772390959204742, 2.373743296044067641, 10.00000000000000000 ) ) ;
#7683 = CIRCLE ( 'NONE', #3395, 9.599999999999997868 ) ;
#7684 = CIRCLE ( 'NONE', #7877, 24.80000000000000071 ) ;
#7685 = CARTESIAN_POINT ( 'NONE',  ( -10.47176928358604364, -8.303818807687074255, 6.857782953271941950E-17 ) ) ;
#7686 = DIRECTION ( 'NONE',  ( -1.000000000000000000, 0.000000000000000000, 0.000000000000000000 ) ) ;
#7687 = ORIENTED_EDGE ( 'NONE', *, *, #2396, .F. ) ;
#7688 = AXIS2_PLACEMENT_3D ( 'NONE', #7080, #722, #4526 ) ;
#7689 = ORIENTED_EDGE ( 'NONE', *, *, #81, .F. ) ;
#7690 = DIRECTION ( 'NONE',  ( -1.000000000000000000, -0.000000000000000000, -0.000000000000000000 ) ) ;
#7691 = DIRECTION ( 'NONE',  ( 0.000000000000000000, 0.000000000000000000, 1.000000000000000000 ) ) ;
#7692 = ORIENTED_EDGE ( 'NONE', *, *, #2318, .F. ) ;
#7693 = DIRECTION ( 'NONE',  ( -1.000000000000000000, 0.000000000000000000, 0.000000000000000000 ) ) ;
#7694 = LINE ( 'NONE', #8622, #351 ) ;
#7695 = CIRCLE ( 'NONE', #11031, 3.500000000000000000 ) ;
#7696 = DIRECTION ( 'NONE',  ( -1.000000000000000000, 0.000000000000000000, -0.000000000000000000 ) ) ;
#7697 = EDGE_CURVE ( 'NONE', #5247, #900, #4664, .T. ) ;
#7698 = CARTESIAN_POINT ( 'NONE',  ( -4.046710180314748939, 10.72208681399755292, 3.747395293195558847E-16 ) ) ;
#7699 = EDGE_CURVE ( 'NONE', #9994, #8613, #7694, .T. ) ;
#7700 = DIRECTION ( 'NONE',  ( 0.000000000000000000, 0.000000000000000000, 1.000000000000000000 ) ) ;
#7701 = VERTEX_POINT ( 'NONE', #9595 ) ;
#7702 = ORIENTED_EDGE ( 'NONE', *, *, #6741, .F. ) ;
#7703 = DIRECTION ( 'NONE',  ( 0.000000000000000000, 1.000000000000000000, 0.000000000000000000 ) ) ;
#7704 = CARTESIAN_POINT ( 'NONE',  ( -5.683926142426734884, 14.39978054689284193, 10.00000000000000000 ) ) ;
#7705 = ORIENTED_EDGE ( 'NONE', *, *, #705, .T. ) ;
#7706 = VECTOR ( 'NONE', #5343, 1000.000000000000000 ) ;
#7707 = CARTESIAN_POINT ( 'NONE',  ( 3.000000000000000888, -21.97702544527762214, 6.779701584702658046 ) ) ;
#7708 = CARTESIAN_POINT ( 'NONE',  ( 0.000000000000000000, 13.62355943574044481, -17.97274125076060258 ) ) ;
#7709 = CARTESIAN_POINT ( 'NONE',  ( 3.000000000000000888, -18.80635025205178579, 13.23915371906949012 ) ) ;
#7710 = VERTEX_POINT ( 'NONE', #8741 ) ;
#7711 = ADVANCED_FACE ( 'NONE', ( #4084 ), #11550, .F. ) ;
#7712 = DIRECTION ( 'NONE',  ( 0.000000000000000000, -0.4999999999999888978, -0.8660254037844452579 ) ) ;
#7713 = EDGE_CURVE ( 'NONE', #1256, #4254, #11308, .T. ) ;
#7714 = CARTESIAN_POINT ( 'NONE',  ( 0.000000000000000000, 6.779701584702736206, 21.97702544527760082 ) ) ;
#7715 = CARTESIAN_POINT ( 'NONE',  ( -9.080917052262540423, 12.68274194616037320, 6.857782953271941950E-17 ) ) ;
#7716 = CIRCLE ( 'NONE', #7116, 24.80000000000000071 ) ;
#7717 = DIRECTION ( 'NONE',  ( 0.000000000000000000, -0.4999999999999887867, -0.8660254037844449249 ) ) ;
#7718 = ORIENTED_EDGE ( 'NONE', *, *, #3483, .T. ) ;
#7719 = DIRECTION ( 'NONE',  ( 0.000000000000000000, 0.000000000000000000, 1.000000000000000000 ) ) ;
#7720 = CYLINDRICAL_SURFACE ( 'NONE', #9784, 22.99899999999999878 ) ;
#7721 = VERTEX_POINT ( 'NONE', #10506 ) ;
#7722 = CARTESIAN_POINT ( 'NONE',  ( -5.318373871714366707, 13.46535835423756566, 10.00000000000000000 ) ) ;
#7723 = DIRECTION ( 'NONE',  ( 0.000000000000000000, 0.6691306063588543518, 0.7431448254773976858 ) ) ;
#7724 = FACE_OUTER_BOUND ( 'NONE', #136, .T. ) ;
#7725 = ADVANCED_FACE ( 'NONE', ( #8862 ), #2122, .T. ) ;
#7726 = DIRECTION ( 'NONE',  ( -1.000000000000000000, 0.000000000000000000, 0.000000000000000000 ) ) ;
#7727 = CARTESIAN_POINT ( 'NONE',  ( 14.54887842078032989, 0.9530482589066729959, 10.00000000000000000 ) ) ;
#7728 = SURFACE_STYLE_USAGE ( .BOTH. , #7600 ) ;
#7729 = DIRECTION ( 'NONE',  ( -1.000000000000000000, -0.000000000000000000, -0.000000000000000000 ) ) ;
#7730 = CARTESIAN_POINT ( 'NONE',  ( 0.000000000000000000, -19.74380051311548456, 11.79560690673865331 ) ) ;
#7731 = ORIENTED_EDGE ( 'NONE', *, *, #5497, .F. ) ;
#7732 = AXIS2_PLACEMENT_3D ( 'NONE', #11095, #6445, #5531 ) ;
#7733 = DIRECTION ( 'NONE',  ( 0.000000000000000000, 0.000000000000000000, -1.000000000000000000 ) ) ;
#7734 = ORIENTED_EDGE ( 'NONE', *, *, #5046, .T. ) ;
#7735 = CARTESIAN_POINT ( 'NONE',  ( 3.000000000000000888, -21.58580335785681115, 6.532525787310899723 ) ) ;
#7736 = CARTESIAN_POINT ( 'NONE',  ( 5.892341078160698409, -4.186101517074010125, 10.00000000000000000 ) ) ;
#7737 = EDGE_CURVE ( 'NONE', #2001, #11239, #5003, .T. ) ;
#7738 = DIRECTION ( 'NONE',  ( -1.000000000000000000, 0.000000000000000000, 0.000000000000000000 ) ) ;
#7739 = AXIS2_PLACEMENT_3D ( 'NONE', #313, #10535, #2153 ) ;
#7740 = CARTESIAN_POINT ( 'NONE',  ( 2.469054641153702434, -10.61194774715159994, 10.00000000000000000 ) ) ;
#7741 = CARTESIAN_POINT ( 'NONE',  ( -5.414455899168758357, -12.47541146648942245, 6.857782953271941950E-17 ) ) ;
#7742 = LINE ( 'NONE', #5109, #11750 ) ;
#7743 = CARTESIAN_POINT ( 'NONE',  ( 1.500000000000000444, 19.10918332567958089, 15.80756504416697439 ) ) ;
#7744 = ORIENTED_EDGE ( 'NONE', *, *, #8688, .T. ) ;
#7745 = EDGE_CURVE ( 'NONE', #8512, #6967, #3100, .T. ) ;
#7746 = CIRCLE ( 'NONE', #11278, 22.99899999999999878 ) ;
#7747 = ORIENTED_EDGE ( 'NONE', *, *, #8931, .F. ) ;
#7748 = LINE ( 'NONE', #341, #11194 ) ;
#7749 = CARTESIAN_POINT ( 'NONE',  ( -3.500000000000000000, 4.286263797015736595E-16, -15.00000000000000000 ) ) ;
#7750 = PRODUCT_DEFINITION_SHAPE ( 'NONE', 'NONE',  #9427 ) ;
#7751 = LINE ( 'NONE', #11486, #11114 ) ;
#7752 = CYLINDRICAL_SURFACE ( 'NONE', #10119, 24.80000000000000071 ) ;
#7753 = CARTESIAN_POINT ( 'NONE',  ( -0.1481022647113159063, -9.773457036294480815, 3.747395293195558847E-16 ) ) ;
#7754 = DIRECTION ( 'NONE',  ( 0.000000000000000000, -0.4067366430758071472, 0.9135454576425979800 ) ) ;
#7755 = ORIENTED_EDGE ( 'NONE', *, *, #11895, .T. ) ;
#7756 = ORIENTED_EDGE ( 'NONE', *, *, #9298, .F. ) ;
#7757 = SHAPE_DEFINITION_REPRESENTATION ( #4926, #8743 ) ;
#7758 = CARTESIAN_POINT ( 'NONE',  ( -1.999398781552333970, 15.23274265415849626, 10.00000000000000000 ) ) ;
#7759 = VERTEX_POINT ( 'NONE', #284 ) ;
#7760 = CARTESIAN_POINT ( 'NONE',  ( 3.000000000000000888, 13.79477846460795831, 18.40266524480593802 ) ) ;
#7761 = FACE_OUTER_BOUND ( 'NONE', #1478, .T. ) ;
#7762 = AXIS2_PLACEMENT_3D ( 'NONE', #6578, #2111, #9580 ) ;
#7763 = DIRECTION ( 'NONE',  ( 0.000000000000000000, 0.000000000000000000, 1.000000000000000000 ) ) ;
#7764 = ORIENTED_EDGE ( 'NONE', *, *, #8315, .T. ) ;
#7765 = DIRECTION ( 'NONE',  ( -1.000000000000000000, -0.000000000000000000, -0.000000000000000000 ) ) ;
#7766 = DIRECTION ( 'NONE',  ( 0.000000000000000000, 0.000000000000000000, 1.000000000000000000 ) ) ;
#7767 = CARTESIAN_POINT ( 'NONE',  ( 12.58137556868280882, 7.823023050434559700, 6.857782953271941950E-17 ) ) ;
#7768 = ADVANCED_FACE ( 'NONE', ( #4023 ), #3110, .F. ) ;
#7769 = ORIENTED_EDGE ( 'NONE', *, *, #1195, .F. ) ;
#7770 = FACE_OUTER_BOUND ( 'NONE', #4498, .T. ) ;
#7771 = VECTOR ( 'NONE', #9867, 1000.000000000000000 ) ;
#7772 = DIRECTION ( 'NONE',  ( -1.000000000000000000, -0.000000000000000000, 0.000000000000000000 ) ) ;
#7773 = ORIENTED_EDGE ( 'NONE', *, *, #2725, .F. ) ;
#7774 = EDGE_CURVE ( 'NONE', #6148, #10264, #10689, .T. ) ;
#7775 = CARTESIAN_POINT ( 'NONE',  ( -9.045553118584756191, -8.482981269325438944, 10.00000000000000000 ) ) ;
#7776 = ADVANCED_FACE ( 'NONE', ( #9655 ), #2301, .T. ) ;
#7777 = CARTESIAN_POINT ( 'NONE',  ( 0.000000000000000000, -12.88318129270165890, -18.51065745848391586 ) ) ;
#7778 = EDGE_CURVE ( 'NONE', #6987, #4516, #1387, .T. ) ;
#7779 =( NAMED_UNIT ( * ) SI_UNIT ( $, .STERADIAN. ) SOLID_ANGLE_UNIT ( ) );
#7780 = ORIENTED_EDGE ( 'NONE', *, *, #5449, .T. ) ;
#7781 = APPLICATION_CONTEXT ( 'automotive_design' ) ;
#7782 = ORIENTED_EDGE ( 'NONE', *, *, #8678, .T. ) ;
#7783 = AXIS2_PLACEMENT_3D ( 'NONE', #6945, #2248, #6827 ) ;
#7784 = LINE ( 'NONE', #10537, #9533 ) ;
#7785 = AXIS2_PLACEMENT_3D ( 'NONE', #11844, #11964, #11904 ) ;
#7786 = DIRECTION ( 'NONE',  ( 1.000000000000000000, 0.000000000000000000, 0.000000000000000000 ) ) ;
#7787 = CARTESIAN_POINT ( 'NONE',  ( -1.124919223378054722, -13.71093750358708796, 10.00000000000000000 ) ) ;
#7788 = DIRECTION ( 'NONE',  ( -1.000000000000000000, 0.000000000000000000, -0.000000000000000000 ) ) ;
#7789 = CARTESIAN_POINT ( 'NONE',  ( -13.29946171776798280, 6.562258890817371793, 3.747395293195558847E-16 ) ) ;
#7790 = DIRECTION ( 'NONE',  ( 0.000000000000000000, 0.000000000000000000, 1.000000000000000000 ) ) ;
#7791 = DIRECTION ( 'NONE',  ( 0.000000000000000000, 0.000000000000000000, 1.000000000000000000 ) ) ;
#7792 = EDGE_LOOP ( 'NONE', ( #3037, #10205, #507, #7951 ) ) ;
#7793 = AXIS2_PLACEMENT_3D ( 'NONE', #9217, #6460, #10195 ) ;
#7794 = CIRCLE ( 'NONE', #6234, 9.599999999999996092 ) ;
#7795 = VERTEX_POINT ( 'NONE', #11663 ) ;
#7796 = ORIENTED_EDGE ( 'NONE', *, *, #9947, .T. ) ;
#7797 = LINE ( 'NONE', #10615, #9681 ) ;
#7798 = CARTESIAN_POINT ( 'NONE',  ( -4.763935748647996959, -4.221771024092342728, 10.00000000000000000 ) ) ;
#7799 = FACE_OUTER_BOUND ( 'NONE', #4865, .T. ) ;
#7800 = CARTESIAN_POINT ( 'NONE',  ( 7.334967666341840165, -8.371827447635059372, 10.00000000000000000 ) ) ;
#7801 = AXIS2_PLACEMENT_3D ( 'NONE', #7013, #4628, #3647 ) ;
#7802 = EDGE_CURVE ( 'NONE', #10397, #6438, #404, .T. ) ;
#7803 = CARTESIAN_POINT ( 'NONE',  ( -11.80455809908225717, -11.41585333555581627, 6.857782953271941950E-17 ) ) ;
#7804 = DIRECTION ( 'NONE',  ( -1.000000000000000000, 0.000000000000000000, 0.000000000000000000 ) ) ;
#7805 = CYLINDRICAL_SURFACE ( 'NONE', #20, 9.599999999999997868 ) ;
#7806 = VERTEX_POINT ( 'NONE', #6714 ) ;
#7807 = EDGE_CURVE ( 'NONE', #6584, #4165, #10450, .T. ) ;
#7808 = ORIENTED_EDGE ( 'NONE', *, *, #10812, .F. ) ;
#7809 = AXIS2_PLACEMENT_3D ( 'NONE', #11013, #9161, #11738 ) ;
#7810 = DIRECTION ( 'NONE',  ( 0.000000000000000000, 0.000000000000000000, 1.000000000000000000 ) ) ;
#7811 = CYLINDRICAL_SURFACE ( 'NONE', #6088, 22.99899999999999878 ) ;
#7812 =( LENGTH_UNIT ( ) NAMED_UNIT ( * ) SI_UNIT ( .MILLI., .METRE. ) );
#7813 = DIRECTION ( 'NONE',  ( 0.000000000000000000, 0.000000000000000000, 1.000000000000000000 ) ) ;
#7814 = EDGE_CURVE ( 'NONE', #3187, #6304, #5439, .T. ) ;
#7815 = CARTESIAN_POINT ( 'NONE',  ( -7.812220363925484357, -5.053636123081432174, 3.747395293195558847E-16 ) ) ;
#7816 = AXIS2_PLACEMENT_3D ( 'NONE', #4996, #2178, #6764 ) ;
#7817 = CIRCLE ( 'NONE', #2547, 24.80000000000000071 ) ;
#7818 = DIRECTION ( 'NONE',  ( 0.000000000000000000, 0.000000000000000000, 1.000000000000000000 ) ) ;
#7819 = ORIENTED_EDGE ( 'NONE', *, *, #9945, .F. ) ;
#7820 = ORIENTED_EDGE ( 'NONE', *, *, #5981, .F. ) ;
#7821 =( NAMED_UNIT ( * ) SI_UNIT ( $, .STERADIAN. ) SOLID_ANGLE_UNIT ( ) );
#7822 = CARTESIAN_POINT ( 'NONE',  ( 8.547432504761534489, 12.33942397201040286, 10.00000000000000000 ) ) ;
#7823 = ORIENTED_EDGE ( 'NONE', *, *, #8315, .F. ) ;
#7824 = DIRECTION ( 'NONE',  ( -0.000000000000000000, -0.000000000000000000, -1.000000000000000000 ) ) ;
#7825 = CARTESIAN_POINT ( 'NONE',  ( 3.000000000000000888, -4.240409074143949297, -22.15038895030653521 ) ) ;
#7826 = AXIS2_PLACEMENT_3D ( 'NONE', #1484, #9811, #561 ) ;
#7827 = DIRECTION ( 'NONE',  ( 1.000000000000000000, 0.000000000000000000, 0.000000000000000000 ) ) ;
#7828 = VECTOR ( 'NONE', #8883, 1000.000000000000000 ) ;
#7829 = ORIENTED_EDGE ( 'NONE', *, *, #11678, .T. ) ;
#7830 = CIRCLE ( 'NONE', #5685, 24.80000000000000071 ) ;
#7831 = DIRECTION ( 'NONE',  ( 0.000000000000000000, 0.000000000000000000, 1.000000000000000000 ) ) ;
#7832 = AXIS2_PLACEMENT_3D ( 'NONE', #11558, #7636, #5011 ) ;
#7833 = DIRECTION ( 'NONE',  ( 0.000000000000000000, 0.2079116908177532641, 0.9781476007338070211 ) ) ;
#7834 = CARTESIAN_POINT ( 'NONE',  ( -11.61414229320030067, -6.453515506896104981, 6.857782953271941950E-17 ) ) ;
#7835 = VERTEX_POINT ( 'NONE', #6222 ) ;
#7836 = CIRCLE ( 'NONE', #6661, 9.599999999999999645 ) ;
#7837 = CARTESIAN_POINT ( 'NONE',  ( 3.000000000000000888, -7.432877647175053504, -21.76479567747249178 ) ) ;
#7838 = AXIS2_PLACEMENT_3D ( 'NONE', #4815, #4695, #34 ) ;
#7839 = ORIENTED_EDGE ( 'NONE', *, *, #8724, .T. ) ;
#7840 = FACE_OUTER_BOUND ( 'NONE', #3090, .T. ) ;
#7841 = AXIS2_PLACEMENT_3D ( 'NONE', #7391, #11134, #1835 ) ;
#7842 = VERTEX_POINT ( 'NONE', #4260 ) ;
#7843 = CARTESIAN_POINT ( 'NONE',  ( -0.3758430365714709454, 11.29677535215814466, 10.00000000000000000 ) ) ;
#7844 = CARTESIAN_POINT ( 'NONE',  ( 0.000000000000000000, -19.43515443678413135, 15.40502424595139530 ) ) ;
#7845 =( LENGTH_UNIT ( ) NAMED_UNIT ( * ) SI_UNIT ( .MILLI., .METRE. ) );
#7846 = AXIS2_PLACEMENT_3D ( 'NONE', #638, #2532, #3463 ) ;
#7848 = VECTOR ( 'NONE', #643, 1000.000000000000000 ) ;
#7847 = DIRECTION ( 'NONE',  ( 0.000000000000000000, 0.9781476007338062439, -0.2079116908177564282 ) ) ;
#7849 = CIRCLE ( 'NONE', #2576, 9.599999999999997868 ) ;
#7850 = CARTESIAN_POINT ( 'NONE',  ( 0.000000000000000000, 0.000000000000000000, 0.000000000000000000 ) ) ;
#7851 = CARTESIAN_POINT ( 'NONE',  ( -4.389456771235332511, 11.66511648340389762, 10.00000000000000000 ) ) ;
#7852 = CARTESIAN_POINT ( 'NONE',  ( 0.000000000000000000, -22.56530478845651544, 4.445336973060782348 ) ) ;
#7853 = CARTESIAN_POINT ( 'NONE',  ( -5.318373871714365819, 13.46535835423756389, 3.747395293195558847E-16 ) ) ;
#7854 = EDGE_CURVE ( 'NONE', #9879, #9423, #9348, .T. ) ;
#7855 = CARTESIAN_POINT ( 'NONE',  ( -10.00000000000000000, 0.000000000000000000, 0.000000000000000000 ) ) ;
#7856 = EDGE_CURVE ( 'NONE', #3870, #1562, #11789, .T. ) ;
#7857 = EDGE_CURVE ( 'NONE', #11802, #8511, #155, .T. ) ;
#7858 = DIRECTION ( 'NONE',  ( 0.000000000000000000, 0.000000000000000000, 1.000000000000000000 ) ) ;
#7859 = VERTEX_POINT ( 'NONE', #7001 ) ;
#7860 = VECTOR ( 'NONE', #1164, 1000.000000000000000 ) ;
#7861 = ORIENTED_EDGE ( 'NONE', *, *, #11230, .F. ) ;
#7862 = CIRCLE ( 'NONE', #9000, 9.599999999999996092 ) ;
#7863 = DIRECTION ( 'NONE',  ( -1.000000000000000000, 0.000000000000000000, -0.000000000000000000 ) ) ;
#7864 = FACE_BOUND ( 'NONE', #8112, .T. ) ;
#7865 = CARTESIAN_POINT ( 'NONE',  ( 3.000000000000000888, -17.35216073792452462, 17.71842311621524146 ) ) ;
#7866 = CARTESIAN_POINT ( 'NONE',  ( -10.03906249502029091, -0.8181230654450249995, 10.00000000000000000 ) ) ;
#7867 = EDGE_CURVE ( 'NONE', #3556, #4653, #11692, .T. ) ;
#7868 = CARTESIAN_POINT ( 'NONE',  ( -16.00307013876014750, -1.840746716621878498, 6.857782953271941950E-17 ) ) ;
#7869 = AXIS2_PLACEMENT_3D ( 'NONE', #8555, #4765, #7443 ) ;
#7870 = CARTESIAN_POINT ( 'NONE',  ( 1.499999999999999556, -11.02759168516730881, -22.21333432029574695 ) ) ;
#7871 = ORIENTED_EDGE ( 'NONE', *, *, #11138, .F. ) ;
#7872 = ORIENTED_EDGE ( 'NONE', *, *, #7162, .T. ) ;
#7873 = VERTEX_POINT ( 'NONE', #7183 ) ;
#7874 = EDGE_CURVE ( 'NONE', #1383, #9137, #7595, .T. ) ;
#7875 = LINE ( 'NONE', #6999, #7643 ) ;
#7876 = DIRECTION ( 'NONE',  ( 0.000000000000000000, 0.000000000000000000, 1.000000000000000000 ) ) ;
#7877 = AXIS2_PLACEMENT_3D ( 'NONE', #1734, #9328, #11289 ) ;
#7878 = CARTESIAN_POINT ( 'NONE',  ( 0.000000000000000000, 0.000000000000000000, -15.00000000000000000 ) ) ;
#7879 = EDGE_CURVE ( 'NONE', #3959, #9646, #7386, .T. ) ;
#7880 = CARTESIAN_POINT ( 'NONE',  ( 8.429646098664187903, -5.822225404888638600, 3.747395293195558847E-16 ) ) ;
#7881 = DIRECTION ( 'NONE',  ( 0.000000000000000000, -0.4067366430757888285, -0.9135454576426059736 ) ) ;
#7882 = VERTEX_POINT ( 'NONE', #3417 ) ;
#7883 = EDGE_LOOP ( 'NONE', ( #4612, #777, #10862, #3194 ) ) ;
#7884 = VECTOR ( 'NONE', #9545, 1000.000000000000000 ) ;
#7885 = DIRECTION ( 'NONE',  ( 0.000000000000000000, -1.000000000000000000, 0.000000000000000000 ) ) ;
#7886 = CARTESIAN_POINT ( 'NONE',  ( -7.327987143158986250, -11.36402271042610224, 10.00000000000000000 ) ) ;
#7887 = EDGE_LOOP ( 'NONE', ( #10121, #3854, #6765, #2092 ) ) ;
#7888 = CARTESIAN_POINT ( 'NONE',  ( 3.000000000000000888, 22.15038895030654942, -4.240409074143872914 ) ) ;
#7889 = CARTESIAN_POINT ( 'NONE',  ( 0.000000000000000000, 0.000000000000000000, 3.000000000000000000 ) ) ;
#7890 = CYLINDRICAL_SURFACE ( 'NONE', #3842, 3.500000000000000000 ) ;
#7891 = ORIENTED_EDGE ( 'NONE', *, *, #8438, .T. ) ;
#7892 = ADVANCED_FACE ( 'NONE', ( #526 ), #11845, .T. ) ;
#7893 = DIRECTION ( 'NONE',  ( -1.000000000000000000, 0.000000000000000000, -0.000000000000000000 ) ) ;
#7894 = CARTESIAN_POINT ( 'NONE',  ( 3.000000000000000888, 0.000000000000000000, 0.000000000000000000 ) ) ;
#7895 = CARTESIAN_POINT ( 'NONE',  ( 0.6097887191948974106, 9.229167205757265791, 6.857782953271941950E-17 ) ) ;
#7896 = VERTEX_POINT ( 'NONE', #10932 ) ;
#7897 = DIRECTION ( 'NONE',  ( 0.000000000000000000, 0.000000000000000000, -1.000000000000000000 ) ) ;
#7898 = CIRCLE ( 'NONE', #1646, 22.99899999999999878 ) ;
#7899 = FACE_OUTER_BOUND ( 'NONE', #1723, .T. ) ;
#7900 = EDGE_CURVE ( 'NONE', #6856, #4609, #9151, .T. ) ;
#7901 = ORIENTED_EDGE ( 'NONE', *, *, #6013, .T. ) ;
#7902 = CARTESIAN_POINT ( 'NONE',  ( -5.773631947676831189, 9.989728373610905265, 10.00000000000000000 ) ) ;
#7903 = ORIENTED_EDGE ( 'NONE', *, *, #1207, .F. ) ;
#7904 = CYLINDRICAL_SURFACE ( 'NONE', #1680, 9.599999999999997868 ) ;
#7905 = VERTEX_POINT ( 'NONE', #2549 ) ;
#7906 = AXIS2_PLACEMENT_3D ( 'NONE', #4981, #3203, #497 ) ;
#7907 = DIRECTION ( 'NONE',  ( -1.000000000000000000, -0.000000000000000000, -0.000000000000000000 ) ) ;
#7908 = CARTESIAN_POINT ( 'NONE',  ( 3.000000000000000888, 2.062268319295869290, -22.90635393027944033 ) ) ;
#7909 = CARTESIAN_POINT ( 'NONE',  ( -6.506554845699742629, -8.196137552274390004, 10.00000000000000000 ) ) ;
#7910 = FILL_AREA_STYLE ('',( #4183 ) ) ;
#7911 = CARTESIAN_POINT ( 'NONE',  ( -13.83044629298881034, 5.462350471645222250, 3.747395293195558847E-16 ) ) ;
#7912 = CARTESIAN_POINT ( 'NONE',  ( 0.000000000000000000, -3.623565124516940461, -24.53384959170461599 ) ) ;
#7913 = CARTESIAN_POINT ( 'NONE',  ( 0.000000000000000000, 0.000000000000000000, 0.000000000000000000 ) ) ;
#7915 = EDGE_CURVE ( 'NONE', #9364, #4270, #11506, .T. ) ;
#7914 = ORIENTED_EDGE ( 'NONE', *, *, #4868, .T. ) ;
#7916 = CYLINDRICAL_SURFACE ( 'NONE', #1872, 9.599999999999994316 ) ;
#7917 = DIRECTION ( 'NONE',  ( 0.000000000000000000, 0.000000000000000000, 1.000000000000000000 ) ) ;
#7918 = EDGE_CURVE ( 'NONE', #5065, #1084, #1735, .T. ) ;
#7919 = CYLINDRICAL_SURFACE ( 'NONE', #7298, 22.99899999999999878 ) ;
#7920 = CARTESIAN_POINT ( 'NONE',  ( 2.004495162477544223, 5.838205294495796949, 10.00000000000000000 ) ) ;
#7921 = AXIS2_PLACEMENT_3D ( 'NONE', #1489, #6873, #2232 ) ;
#7922 = CARTESIAN_POINT ( 'NONE',  ( 0.7062845326066684581, -10.79445016380498501, 6.857782953271941950E-17 ) ) ;
#7923 = FACE_OUTER_BOUND ( 'NONE', #1576, .T. ) ;
#7924 = CYLINDRICAL_SURFACE ( 'NONE', #4697, 9.599999999999997868 ) ;
#7925 = ADVANCED_FACE ( 'NONE', ( #1568 ), #6286, .T. ) ;
#7926 = EDGE_LOOP ( 'NONE', ( #905, #12106, #11347, #5323 ) ) ;
#7927 = VERTEX_POINT ( 'NONE', #6104 ) ;
#7928 = ORIENTED_EDGE ( 'NONE', *, *, #8556, .T. ) ;
#7929 = EDGE_CURVE ( 'NONE', #6719, #9406, #5648, .T. ) ;
#7930 = DIRECTION ( 'NONE',  ( 0.000000000000000000, 0.000000000000000000, 1.000000000000000000 ) ) ;
#7931 = EDGE_CURVE ( 'NONE', #9213, #2104, #5058, .T. ) ;
#7932 = DIRECTION ( 'NONE',  ( 0.000000000000000000, 0.8090169943749445647, 0.5877852522924771339 ) ) ;
#7933 = FACE_OUTER_BOUND ( 'NONE', #8263, .T. ) ;
#7934 = EDGE_CURVE ( 'NONE', #2892, #11802, #6035, .T. ) ;
#7935 = CARTESIAN_POINT ( 'NONE',  ( -9.680665087125342794, -7.686621967951971612, 3.747395293195558847E-16 ) ) ;
#7936 = CARTESIAN_POINT ( 'NONE',  ( 0.000000000000000000, -6.168200451485919444, 24.02068490260611000 ) ) ;
#7937 = CIRCLE ( 'NONE', #2081, 22.99900000000000233 ) ;
#7938 = CARTESIAN_POINT ( 'NONE',  ( 0.000000000000000000, -6.668524164681792321, 23.88662356770113249 ) ) ;
#7939 = ORIENTED_EDGE ( 'NONE', *, *, #207, .F. ) ;
#7940 = ORIENTED_EDGE ( 'NONE', *, *, #11812, .F. ) ;
#7941 = CARTESIAN_POINT ( 'NONE',  ( 12.58137556868281237, 7.823023050435613968, 10.00000000000000000 ) ) ;
#7942 = ORIENTED_EDGE ( 'NONE', *, *, #1061, .T. ) ;
#7943 = DIRECTION ( 'NONE',  ( 0.000000000000000000, 0.000000000000000000, -1.000000000000000000 ) ) ;
#7944 = DIRECTION ( 'NONE',  ( -1.000000000000000000, 0.000000000000000000, 0.000000000000000000 ) ) ;
#7945 = UNCERTAINTY_MEASURE_WITH_UNIT (LENGTH_MEASURE( 1.000000000000000082E-05 ), #374, 'distance_accuracy_value', 'NONE');
#7946 = LINE ( 'NONE', #2136, #10677 ) ;
#7947 = ORIENTED_EDGE ( 'NONE', *, *, #10436, .F. ) ;
#7948 = CARTESIAN_POINT ( 'NONE',  ( 3.000000000000000888, 0.000000000000000000, 0.000000000000000000 ) ) ;
#7949 = CARTESIAN_POINT ( 'NONE',  ( 0.000000000000000000, 0.000000000000000000, 0.000000000000000000 ) ) ;
#7950 = CARTESIAN_POINT ( 'NONE',  ( -9.977213461302312680, -1.645879626164740817, 6.857782953271941950E-17 ) ) ;
#7951 = ORIENTED_EDGE ( 'NONE', *, *, #2240, .T. ) ;
#7952 = CARTESIAN_POINT ( 'NONE',  ( 3.000000000000000888, 15.64281154287620446, -16.85990652506883691 ) ) ;
#7953 = DIRECTION ( 'NONE',  ( 0.000000000000000000, 0.000000000000000000, 1.000000000000000000 ) ) ;
#7954 = ORIENTED_EDGE ( 'NONE', *, *, #9546, .T. ) ;
#7955 = EDGE_CURVE ( 'NONE', #11767, #2929, #8188, .T. ) ;
#7956 = CARTESIAN_POINT ( 'NONE',  ( 9.962304844536470583, 3.945508033568877249, 10.00000000000000000 ) ) ;
#7957 = CARTESIAN_POINT ( 'NONE',  ( 0.000000000000000000, -24.77821629063820907, -1.039229259764747004 ) ) ;
#7958 = AXIS2_PLACEMENT_3D ( 'NONE', #2852, #4752, #11351 ) ;
#7959 = DIRECTION ( 'NONE',  ( 1.000000000000000000, 0.000000000000000000, -0.000000000000000000 ) ) ;
#7960 = EDGE_CURVE ( 'NONE', #10168, #10729, #11113, .T. ) ;
#7961 = FACE_OUTER_BOUND ( 'NONE', #10220, .T. ) ;
#7962 = CARTESIAN_POINT ( 'NONE',  ( 5.247589697392150754, -6.187652788349034871, 10.00000000000000000 ) ) ;
#7963 = CIRCLE ( 'NONE', #5630, 24.80000000000000071 ) ;
#7964 = DIRECTION ( 'NONE',  ( -1.000000000000000000, -0.000000000000000000, -0.000000000000000000 ) ) ;
#7965 = CARTESIAN_POINT ( 'NONE',  ( -11.92955594661033203, -2.174140050202131302, 3.747395293195558847E-16 ) ) ;
#7966 = DIRECTION ( 'NONE',  ( -1.000000000000000000, -0.000000000000000000, 0.000000000000000000 ) ) ;
#7967 = ORIENTED_EDGE ( 'NONE', *, *, #4065, .T. ) ;
#7968 = FACE_OUTER_BOUND ( 'NONE', #7410, .T. ) ;
#7969 = ORIENTED_EDGE ( 'NONE', *, *, #7307, .T. ) ;
#7970 = AXIS2_PLACEMENT_3D ( 'NONE', #3660, #11371, #853 ) ;
#7971 = CARTESIAN_POINT ( 'NONE',  ( 8.000000000000000000, 0.000000000000000000, 0.000000000000000000 ) ) ;
#7972 = ORIENTED_EDGE ( 'NONE', *, *, #4211, .T. ) ;
#7973 = CARTESIAN_POINT ( 'NONE',  ( 3.000000000000000888, -15.64281154287585807, -16.85990652506916021 ) ) ;
#7974 = DIRECTION ( 'NONE',  ( 0.000000000000000000, 0.000000000000000000, 1.000000000000000000 ) ) ;
#7975 = CARTESIAN_POINT ( 'NONE',  ( 3.666996827460253350, 4.772409917195344242, 10.00000000000000000 ) ) ;
#7976 = CARTESIAN_POINT ( 'NONE',  ( -0.1504880127286837288, 9.287785325659760005, 6.857782953271941950E-17 ) ) ;
#7977 = FACE_OUTER_BOUND ( 'NONE', #11188, .T. ) ;
#7978 = VECTOR ( 'NONE', #5994, 1000.000000000000000 ) ;
#7979 = CARTESIAN_POINT ( 'NONE',  ( 3.000000000000000888, 15.13242714128143440, -17.31945870441131419 ) ) ;
#7980 = ORIENTED_EDGE ( 'NONE', *, *, #330, .F. ) ;
#7981 = ORIENTED_EDGE ( 'NONE', *, *, #6105, .T. ) ;
#7982 = ORIENTED_EDGE ( 'NONE', *, *, #3289, .F. ) ;
#7983 = CARTESIAN_POINT ( 'NONE',  ( 12.25096627321952170, 6.291700371256734314, 10.00000000000000000 ) ) ;
#7984 = CIRCLE ( 'NONE', #8196, 24.80000000000000071 ) ;
#7985 =( NAMED_UNIT ( * ) SI_UNIT ( $, .STERADIAN. ) SOLID_ANGLE_UNIT ( ) );
#7986 = DIRECTION ( 'NONE',  ( 0.000000000000000000, 0.9781476007338062439, -0.2079116908177564282 ) ) ;
#7987 = CARTESIAN_POINT ( 'NONE',  ( 7.527773320476327079, 0.8933511214758176333, 3.747395293195558847E-16 ) ) ;
#7988 = ADVANCED_FACE ( 'NONE', ( #8055 ), #3650, .T. ) ;
#7989 = CYLINDRICAL_SURFACE ( 'NONE', #5300, 9.599999999999997868 ) ;
#7990 = EDGE_CURVE ( 'NONE', #246, #2892, #9748, .T. ) ;
#7991 = DIRECTION ( 'NONE',  ( -1.000000000000000000, -0.000000000000000000, 0.000000000000000000 ) ) ;
#7992 = AXIS2_PLACEMENT_3D ( 'NONE', #9594, #43, #5679 ) ;
#7993 = EDGE_LOOP ( 'NONE', ( #11139, #5207, #9828, #3264 ) ) ;
#7994 = EDGE_LOOP ( 'NONE', ( #11706, #10429, #7481, #7773 ) ) ;
#7995 = CARTESIAN_POINT ( 'NONE',  ( 10.35108484788239203, -9.702746953904565430, 10.00000000000000000 ) ) ;
#7996 = ADVANCED_FACE ( 'NONE', ( #7432 ), #5482, .T. ) ;
#7997 = CIRCLE ( 'NONE', #11714, 22.99900000000000233 ) ;
#7998 = ORIENTED_EDGE ( 'NONE', *, *, #9453, .F. ) ;
#7999 = DIRECTION ( 'NONE',  ( -1.000000000000000000, 0.000000000000000000, 0.000000000000000000 ) ) ;
#8000 = CARTESIAN_POINT ( 'NONE',  ( 3.000000000000000888, 0.000000000000000000, 0.000000000000000000 ) ) ;
#8001 = CYLINDRICAL_SURFACE ( 'NONE', #2331, 22.99899999999999878 ) ;
#8002 = DIRECTION ( 'NONE',  ( 0.000000000000000000, 0.000000000000000000, -1.000000000000000000 ) ) ;
#8003 = ORIENTED_EDGE ( 'NONE', *, *, #11435, .T. ) ;
#8004 = CARTESIAN_POINT ( 'NONE',  ( 1.500000000000000444, -19.43515443678392529, -15.40502424595165110 ) ) ;
#8005 = VECTOR ( 'NONE', #3831, 1000.000000000000000 ) ;
#8006 = CARTESIAN_POINT ( 'NONE',  ( 3.000000000000000888, 0.000000000000000000, 0.000000000000000000 ) ) ;
#8007 = CARTESIAN_POINT ( 'NONE',  ( 10.90031251054715966, 4.301772984117409493, 6.857782953271941950E-17 ) ) ;
#8008 = EDGE_CURVE ( 'NONE', #11191, #1896, #4470, .T. ) ;
#8009 = APPLICATION_CONTEXT ( 'automotive_design' ) ;
#8010 = DIRECTION ( 'NONE',  ( 1.000000000000000000, 0.000000000000000000, 0.000000000000000000 ) ) ;
#8011 = CARTESIAN_POINT ( 'NONE',  ( 0.000000000000000000, -4.240409074143949297, -22.15038895030653521 ) ) ;
#8012 = AXIS2_PLACEMENT_3D ( 'NONE', #4923, #1253, #6866 ) ;
#8013 = ORIENTED_EDGE ( 'NONE', *, *, #2385, .T. ) ;
#8014 = CARTESIAN_POINT ( 'NONE',  ( -2.069312577552833154, -12.54440658741724235, 10.00000000000000000 ) ) ;
#8015 = VECTOR ( 'NONE', #2404, 1000.000000000000000 ) ;
#8016 = ORIENTED_EDGE ( 'NONE', *, *, #4269, .T. ) ;
#8017 = EDGE_CURVE ( 'NONE', #11921, #8297, #1813, .T. ) ;
#8018 = CARTESIAN_POINT ( 'NONE',  ( 3.000000000000000888, 0.000000000000000000, 0.000000000000000000 ) ) ;
#8019 = PLANE ( 'NONE',  #3768 ) ;
#8020 = DIRECTION ( 'NONE',  ( -1.000000000000000000, 0.000000000000000000, -0.000000000000000000 ) ) ;
#8021 = ORIENTED_EDGE ( 'NONE', *, *, #7807, .T. ) ;
#8022 = DIRECTION ( 'NONE',  ( 0.000000000000000000, 0.000000000000000000, 1.000000000000000000 ) ) ;
#8023 = CARTESIAN_POINT ( 'NONE',  ( 3.000000000000000888, 15.64281154287597353, 16.85990652506905363 ) ) ;
#8024 = CARTESIAN_POINT ( 'NONE',  ( -9.352287007200070335, 3.176141031410558924, 10.00000000000000000 ) ) ;
#8025 = AXIS2_PLACEMENT_3D ( 'NONE', #1667, #10290, #1010 ) ;
#8026 = ADVANCED_FACE ( 'NONE', ( #11965 ), #10258, .T. ) ;
#8027 = FACE_OUTER_BOUND ( 'NONE', #10994, .T. ) ;
#8028 = CARTESIAN_POINT ( 'NONE',  ( 13.03626601087042758, 4.193914020170396384, 3.747395293195558847E-16 ) ) ;
#8029 = AXIS2_PLACEMENT_3D ( 'NONE', #3616, #789, #11922 ) ;
#8030 = DIRECTION ( 'NONE',  ( -1.000000000000000000, -0.000000000000000000, 0.000000000000000000 ) ) ;
#8031 = ORIENTED_EDGE ( 'NONE', *, *, #462, .F. ) ;
#8032 = CARTESIAN_POINT ( 'NONE',  ( 3.000000000000000888, 0.000000000000000000, 0.000000000000000000 ) ) ;
#8033 = ORIENTED_EDGE ( 'NONE', *, *, #7356, .T. ) ;
#8034 = EDGE_CURVE ( 'NONE', #8709, #5010, #3892, .T. ) ;
#8035 = DIRECTION ( 'NONE',  ( -1.000000000000000000, 0.000000000000000000, 0.000000000000000000 ) ) ;
#8036 = AXIS2_PLACEMENT_3D ( 'NONE', #9341, #9222, #11116 ) ;
#8037 = FACE_OUTER_BOUND ( 'NONE', #5203, .T. ) ;
#8038 = ORIENTED_EDGE ( 'NONE', *, *, #2927, .F. ) ;
#8039 = CIRCLE ( 'NONE', #817, 24.80000000000000071 ) ;
#8040 = CIRCLE ( 'NONE', #1784, 22.99899999999999878 ) ;
#8041 = CARTESIAN_POINT ( 'NONE',  ( 0.000000000000000000, 0.000000000000000000, 0.000000000000000000 ) ) ;
#8042 = CARTESIAN_POINT ( 'NONE',  ( 3.000000000000000888, 0.3433949777331667397, 22.99643626497956816 ) ) ;
#8043 = DIRECTION ( 'NONE',  ( -1.000000000000000000, -0.000000000000000000, 0.000000000000000000 ) ) ;
#8044 = CARTESIAN_POINT ( 'NONE',  ( -6.266017822847494756, 10.86399168115690728, 6.857782953271941950E-17 ) ) ;
#8045 = SURFACE_SIDE_STYLE ('',( #9885 ) ) ;
#8046 = AXIS2_PLACEMENT_3D ( 'NONE', #1541, #2339, #8094 ) ;
#8047 = CARTESIAN_POINT ( 'NONE',  ( 3.000000000000000888, -20.78471918669866270, 8.753070780933086326 ) ) ;
#8048 = EDGE_LOOP ( 'NONE', ( #3391, #10515, #3819, #9762 ) ) ;
#8049 = CIRCLE ( 'NONE', #7428, 9.599999999999997868 ) ;
#8050 = VERTEX_POINT ( 'NONE', #2731 ) ;
#8051 = VERTEX_POINT ( 'NONE', #10126 ) ;
#8052 = CARTESIAN_POINT ( 'NONE',  ( -15.05755265055531389, -0.4891349978715465729, 10.00000000000000000 ) ) ;
#8053 = AXIS2_PLACEMENT_3D ( 'NONE', #12004, #11149, #5401 ) ;
#8054 = CIRCLE ( 'NONE', #10007, 24.80000000000000071 ) ;
#8055 = FACE_OUTER_BOUND ( 'NONE', #5473, .T. ) ;
#8056 = VECTOR ( 'NONE', #8035, 1000.000000000000000 ) ;
#8057 = CARTESIAN_POINT ( 'NONE',  ( 0.000000000000000000, 9.667200211209820537, 20.86861857134737619 ) ) ;
#8058 = CARTESIAN_POINT ( 'NONE',  ( -6.925491926711623059, 5.292860106065907289, 3.747395293195558847E-16 ) ) ;
#8059 = CARTESIAN_POINT ( 'NONE',  ( 3.000000000000000888, -19.43515443678412424, 15.40502424595139175 ) ) ;
#8060 = CARTESIAN_POINT ( 'NONE',  ( 0.000000000000000000, 24.02068490260621303, -6.168200451485523317 ) ) ;
#8061 = ORIENTED_EDGE ( 'NONE', *, *, #6013, .F. ) ;
#8062 = VECTOR ( 'NONE', #839, 1000.000000000000000 ) ;
#8063 = VERTEX_POINT ( 'NONE', #5551 ) ;
#8064 = ORIENTED_EDGE ( 'NONE', *, *, #2699, .F. ) ;
#8065 = EDGE_CURVE ( 'NONE', #4775, #4413, #759, .T. ) ;
#8066 = LINE ( 'NONE', #1458, #3975 ) ;
#8067 = AXIS2_PLACEMENT_3D ( 'NONE', #1558, #4250, #758 ) ;
#8068 = CARTESIAN_POINT ( 'NONE',  ( 3.000000000000000888, -18.51065745848368849, -12.88318129270198042 ) ) ;
#8069 = DIRECTION ( 'NONE',  ( -1.000000000000000000, 0.000000000000000000, -0.000000000000000000 ) ) ;
#8070 = CARTESIAN_POINT ( 'NONE',  ( 0.000000000000000000, 0.000000000000000000, 0.000000000000000000 ) ) ;
#8071 = VERTEX_POINT ( 'NONE', #8362 ) ;
#8072 = CIRCLE ( 'NONE', #3390, 22.99899999999999523 ) ;
#8073 = CYLINDRICAL_SURFACE ( 'NONE', #11981, 24.80000000000000071 ) ;
#8074 = EDGE_CURVE ( 'NONE', #8486, #7265, #4691, .T. ) ;
#8075 = DIRECTION ( 'NONE',  ( 0.000000000000000000, -0.5000000000000072164, 0.8660254037844345998 ) ) ;
#8076 = CARTESIAN_POINT ( 'NONE',  ( -2.764021070441483374, -10.29567250283335689, 6.857782953271941950E-17 ) ) ;
#8077 = VECTOR ( 'NONE', #8810, 1000.000000000000000 ) ;
#8078 = CARTESIAN_POINT ( 'NONE',  ( 0.000000000000000000, 0.000000000000000000, 0.000000000000000000 ) ) ;
#8079 = DIRECTION ( 'NONE',  ( -1.000000000000000000, -0.000000000000000000, -0.000000000000000000 ) ) ;
#8080 = ORIENTED_EDGE ( 'NONE', *, *, #9683, .T. ) ;
#8081 = CIRCLE ( 'NONE', #451, 19.00000000000000000 ) ;
#8082 = ORIENTED_EDGE ( 'NONE', *, *, #8115, .T. ) ;
#8083 = CARTESIAN_POINT ( 'NONE',  ( 7.261170810407329590, -1.543028577657542311, 10.00000000000000000 ) ) ;
#8084 = EDGE_CURVE ( 'NONE', #8218, #10492, #2796, .T. ) ;
#8085 = ORIENTED_EDGE ( 'NONE', *, *, #9121, .F. ) ;
#8086 = CARTESIAN_POINT ( 'NONE',  ( 0.0002901587068754535662, -4.749354241797641762, 5.000000000000000000 ) ) ;
#8087 = LINE ( 'NONE', #4288, #10147 ) ;
#8088 = EDGE_LOOP ( 'NONE', ( #5494, #11316, #2750, #1767 ) ) ;
#8089 = ADVANCED_FACE ( 'NONE', ( #3778 ), #12025, .T. ) ;
#8090 = LINE ( 'NONE', #7337, #6790 ) ;
#8091 = CARTESIAN_POINT ( 'NONE',  ( 3.000000000000000888, 0.000000000000000000, 0.000000000000000000 ) ) ;
#8092 = CARTESIAN_POINT ( 'NONE',  ( -9.820986981723351050, 1.626514086989862662, 10.00000000000000000 ) ) ;
#8093 = CIRCLE ( 'NONE', #7290, 5.000000000000000000 ) ;
#8094 = DIRECTION ( 'NONE',  ( 0.000000000000000000, 0.000000000000000000, 1.000000000000000000 ) ) ;
#8095 = CARTESIAN_POINT ( 'NONE',  ( 12.25096627321951814, 6.291700371256212065, 3.747395293195558847E-16 ) ) ;
#8096 = DIRECTION ( 'NONE',  ( -1.000000000000000000, 0.000000000000000000, 0.000000000000000000 ) ) ;
#8097 = ORIENTED_EDGE ( 'NONE', *, *, #5778, .F. ) ;
#8098 = DIRECTION ( 'NONE',  ( 1.000000000000000000, 0.000000000000000000, 0.000000000000000000 ) ) ;
#8099 = ORIENTED_EDGE ( 'NONE', *, *, #11699, .F. ) ;
#8100 = CARTESIAN_POINT ( 'NONE',  ( -6.036922680726758195, -0.4347383792561972382, 3.747395293195558847E-16 ) ) ;
#8101 = AXIS2_PLACEMENT_3D ( 'NONE', #6802, #2221, #11760 ) ;
#8102 = EDGE_CURVE ( 'NONE', #11246, #4392, #8809, .T. ) ;
#8103 = DIRECTION ( 'NONE',  ( -1.000000000000000000, -0.000000000000000000, -0.000000000000000000 ) ) ;
#8104 = PRESENTATION_STYLE_ASSIGNMENT (( #694 ) ) ;
#8105 = ORIENTED_EDGE ( 'NONE', *, *, #3066, .T. ) ;
#8106 = CARTESIAN_POINT ( 'NONE',  ( 0.000000000000000000, 0.000000000000000000, 0.000000000000000000 ) ) ;
#8107 = CARTESIAN_POINT ( 'NONE',  ( 3.000000000000000888, -20.41249101028205004, -9.589108953448107542 ) ) ;
#8108 = CARTESIAN_POINT ( 'NONE',  ( 5.531377455021724288, -0.3672033614207039776, 10.00000000000000000 ) ) ;
#8109 = CARTESIAN_POINT ( 'NONE',  ( -4.368568794346921358, -9.638580752213396607, 6.857782953271941950E-17 ) ) ;
#8110 = DIRECTION ( 'NONE',  ( -1.000000000000000000, -0.000000000000000000, -0.000000000000000000 ) ) ;
#8111 = DIRECTION ( 'NONE',  ( 0.000000000000000000, 0.000000000000000000, 1.000000000000000000 ) ) ;
#8112 = EDGE_LOOP ( 'NONE', ( #1660, #5077 ) ) ;
#8113 = ORIENTED_EDGE ( 'NONE', *, *, #10812, .T. ) ;
#8114 = ORIENTED_EDGE ( 'NONE', *, *, #2951, .F. ) ;
#8115 = EDGE_CURVE ( 'NONE', #1170, #10578, #9666, .T. ) ;
#8116 = CARTESIAN_POINT ( 'NONE',  ( -13.25288834650809910, -7.646628085889272342, 10.00000000000000000 ) ) ;
#8117 = CARTESIAN_POINT ( 'NONE',  ( 0.000000000000000000, -22.83456483164690809, 2.745295967525920311 ) ) ;
#8118 = DIRECTION ( 'NONE',  ( 0.000000000000000000, 0.000000000000000000, 1.000000000000000000 ) ) ;
#8119 = AXIS2_PLACEMENT_3D ( 'NONE', #10675, #8782, #11532 ) ;
#8120 = EDGE_CURVE ( 'NONE', #7087, #3509, #9552, .T. ) ;
#8121 = CARTESIAN_POINT ( 'NONE',  ( -3.432991321284826647, 4.402131891631369420, 3.747395293195558847E-16 ) ) ;
#8122 = LINE ( 'NONE', #4509, #11936 ) ;
#8123 = DIRECTION ( 'NONE',  ( -1.000000000000000000, 0.000000000000000000, 0.000000000000000000 ) ) ;
#8124 = ORIENTED_EDGE ( 'NONE', *, *, #5239, .T. ) ;
#8125 = VERTEX_POINT ( 'NONE', #3061 ) ;
#8126 = AXIS2_PLACEMENT_3D ( 'NONE', #751, #4486, #8285 ) ;
#8127 = ITEM_DEFINED_TRANSFORMATION ( 'NONE', 'NONE', #3934,  #8474 ) ;
#8128 = ORIENTED_EDGE ( 'NONE', *, *, #5160, .F. ) ;
#8129 = FACE_OUTER_BOUND ( 'NONE', #1698, .T. ) ;
#8130 = CARTESIAN_POINT ( 'NONE',  ( 0.000000000000000000, 11.67026512804547345, 19.29833442572363822 ) ) ;
#8131 = DIRECTION ( 'NONE',  ( -1.000000000000000000, -0.000000000000000000, 0.000000000000000000 ) ) ;
#8132 = ORIENTED_EDGE ( 'NONE', *, *, #5345, .F. ) ;
#8133 = CARTESIAN_POINT ( 'NONE',  ( 0.000000000000000000, -16.85990652506910692, 15.64281154287591669 ) ) ;
#8134 = AXIS2_PLACEMENT_3D ( 'NONE', #11516, #1297, #2274 ) ;
#8135 = CARTESIAN_POINT ( 'NONE',  ( 0.000000000000000000, -9.039786367038983528, 21.14796121233193560 ) ) ;
#8136 = CARTESIAN_POINT ( 'NONE',  ( -4.859750766526011567, 4.557676925202717833, 6.857782953271941950E-17 ) ) ;
#8137 = LINE ( 'NONE', #10218, #6269 ) ;
#8138 = EDGE_LOOP ( 'NONE', ( #7533, #9159, #6712, #11645 ) ) ;
#8139 = CARTESIAN_POINT ( 'NONE',  ( 3.000000000000000888, 22.83456483164689033, 2.745295967526073078 ) ) ;
#8140 = ORIENTED_EDGE ( 'NONE', *, *, #1738, .F. ) ;
#8141 = ORIENTED_EDGE ( 'NONE', *, *, #2578, .F. ) ;
#8142 = AXIS2_PLACEMENT_3D ( 'NONE', #5016, #8877, #8752 ) ;
#8143 = CARTESIAN_POINT ( 'NONE',  ( -8.834572391846261752, 1.442725564903824420, 10.00000000000000000 ) ) ;
#8144 = ORIENTED_EDGE ( 'NONE', *, *, #6513, .T. ) ;
#8145 = CARTESIAN_POINT ( 'NONE',  ( 1.500000000000000444, 4.135161237383916166, -24.45282072769597193 ) ) ;
#8146 = ADVANCED_FACE ( 'NONE', ( #5939 ), #4161, .T. ) ;
#8147 = DIRECTION ( 'NONE',  ( 0.000000000000000000, 0.000000000000000000, -1.000000000000000000 ) ) ;
#8148 = DIRECTION ( 'NONE',  ( -1.000000000000000000, 0.000000000000000000, -0.000000000000000000 ) ) ;
#8149 = CARTESIAN_POINT ( 'NONE',  ( 2.919619825260427071, -7.400844473264730716, 10.00000000000000000 ) ) ;
#8150 = FACE_OUTER_BOUND ( 'NONE', #9188, .T. ) ;
#8151 = PRODUCT_DEFINITION ( 'UNKNOWN', '', #4318, #9162 ) ;
#8152 = CYLINDRICAL_SURFACE ( 'NONE', #7425, 9.599999999999997868 ) ;
#8153 = ORIENTED_EDGE ( 'NONE', *, *, #1520, .F. ) ;
#8154 = CARTESIAN_POINT ( 'NONE',  ( 3.000000000000000888, 2.811977935938088535, -22.37663021667340857 ) ) ;
#8155 = EDGE_CURVE ( 'NONE', #6438, #3896, #11896, .T. ) ;
#8156 = ORIENTED_EDGE ( 'NONE', *, *, #8650, .F. ) ;
#8157 = EDGE_CURVE ( 'NONE', #10684, #3630, #3004, .T. ) ;
#8158 = CARTESIAN_POINT ( 'NONE',  ( -5.315861670734002509, 2.363279591655833567, 3.747395293195558847E-16 ) ) ;
#8159 = CYLINDRICAL_SURFACE ( 'NONE', #99, 24.80000000000000071 ) ;
#8160 = EDGE_LOOP ( 'NONE', ( #879, #6425, #4761, #6215 ) ) ;
#8161 = AXIS2_PLACEMENT_3D ( 'NONE', #5968, #4245, #8728 ) ;
#8162 = CYLINDRICAL_SURFACE ( 'NONE', #10307, 9.599999999999997868 ) ;
#8163 = CARTESIAN_POINT ( 'NONE',  ( 3.000000000000000888, 22.15038895030649257, 4.240409074144170454 ) ) ;
#8164 = CARTESIAN_POINT ( 'NONE',  ( 4.346347989804005607, 4.041826679702273495, 10.00000000000000000 ) ) ;
#8165 = CARTESIAN_POINT ( 'NONE',  ( -3.406233159845096559, 11.94786423299364486, 6.857782953271941950E-17 ) ) ;
#8166 = FACE_OUTER_BOUND ( 'NONE', #11925, .T. ) ;
#8167 = DIRECTION ( 'NONE',  ( 1.000000000000000000, -0.000000000000000000, 0.000000000000000000 ) ) ;
#8168 = ORIENTED_EDGE ( 'NONE', *, *, #4598, .F. ) ;
#8169 = AXIS2_PLACEMENT_3D ( 'NONE', #11585, #5956, #3202 ) ;
#8170 = ORIENTED_EDGE ( 'NONE', *, *, #3662, .T. ) ;
#8171 = ORIENTED_EDGE ( 'NONE', *, *, #9496, .F. ) ;
#8172 = CARTESIAN_POINT ( 'NONE',  ( 3.885483365683945145, 13.62125166200965332, 10.00000000000000000 ) ) ;
#8173 = CARTESIAN_POINT ( 'NONE',  ( 3.000000000000000888, 16.85990652506900389, 15.64281154287603215 ) ) ;
#8174 = EDGE_CURVE ( 'NONE', #1307, #277, #4032, .T. ) ;
#8175 = DIRECTION ( 'NONE',  ( -1.000000000000000000, 0.000000000000000000, -0.000000000000000000 ) ) ;
#8176 = VECTOR ( 'NONE', #6649, 1000.000000000000000 ) ;
#8177 = AXIS2_PLACEMENT_3D ( 'NONE', #10875, #8918, #2486 ) ;
#8178 = CARTESIAN_POINT ( 'NONE',  ( 7.402789038520869447, -0.9464297003978341394, 3.747395293195558847E-16 ) ) ;
#8179 = EDGE_CURVE ( 'NONE', #7150, #8200, #163, .T. ) ;
#8180 = CARTESIAN_POINT ( 'NONE',  ( 0.000000000000000000, 0.000000000000000000, 0.000000000000000000 ) ) ;
#8181 = ORIENTED_EDGE ( 'NONE', *, *, #9094, .F. ) ;
#8182 = CARTESIAN_POINT ( 'NONE',  ( 0.000000000000000000, -1.039229259764318680, -24.77821629063823394 ) ) ;
#8183 = VERTEX_POINT ( 'NONE', #4894 ) ;
#8184 = ADVANCED_FACE ( 'NONE', ( #1401 ), #4094, .T. ) ;
#8185 = APPLICATION_PROTOCOL_DEFINITION ( 'draft international standard', 'automotive_design', 1998, #11146 ) ;
#8186 = VERTEX_POINT ( 'NONE', #10584 ) ;
#8187 = LINE ( 'NONE', #2560, #11011 ) ;
#8188 = CIRCLE ( 'NONE', #8589, 22.99899999999999878 ) ;
#8189 = CIRCLE ( 'NONE', #3478, 9.599999999999999645 ) ;
#8190 = DIRECTION ( 'NONE',  ( 0.000000000000000000, 0.000000000000000000, 1.000000000000000000 ) ) ;
#8191 = EDGE_CURVE ( 'NONE', #2147, #9529, #10700, .T. ) ;
#8192 = CARTESIAN_POINT ( 'NONE',  ( 1.499999999999999556, -24.45282072769597903, -4.135161237383830901 ) ) ;
#8193 = DIRECTION ( 'NONE',  ( 0.000000000000000000, 0.000000000000000000, 1.000000000000000000 ) ) ;
#8194 = CARTESIAN_POINT ( 'NONE',  ( 3.000000000000000888, 17.97274125076092233, -13.62355943574001671 ) ) ;
#8195 = CARTESIAN_POINT ( 'NONE',  ( -0.5113267480521395125, 6.289062763288773894, 6.857782953271941950E-17 ) ) ;
#8196 = AXIS2_PLACEMENT_3D ( 'NONE', #11178, #5603, #10191 ) ;
#8197 = DIRECTION ( 'NONE',  ( -1.000000000000000000, 0.000000000000000000, -0.000000000000000000 ) ) ;
#8198 = DIRECTION ( 'NONE',  ( 0.000000000000000000, 0.000000000000000000, 1.000000000000000000 ) ) ;
#8199 = VERTEX_POINT ( 'NONE', #1334 ) ;
#8200 = VERTEX_POINT ( 'NONE', #8750 ) ;
#8201 = VECTOR ( 'NONE', #141, 1000.000000000000000 ) ;
#8202 = CARTESIAN_POINT ( 'NONE',  ( 0.9209971296404340091, -6.773236541304583191, 10.00000000000000000 ) ) ;
#8203 = CIRCLE ( 'NONE', #3907, 9.599999999999999645 ) ;
#8204 = ORIENTED_EDGE ( 'NONE', *, *, #1797, .T. ) ;
#8205 = CYLINDRICAL_SURFACE ( 'NONE', #311, 9.599999999999997868 ) ;
#8206 = VERTEX_POINT ( 'NONE', #2078 ) ;
#8207 = AXIS2_PLACEMENT_3D ( 'NONE', #5730, #11908, #1015 ) ;
#8208 = CARTESIAN_POINT ( 'NONE',  ( -4.500000000000000000, 0.4999999999999998890, 0.000000000000000000 ) ) ;
#8209 = LINE ( 'NONE', #7217, #881 ) ;
#8210 = CARTESIAN_POINT ( 'NONE',  ( 0.6279411196271856843, -4.781877258324073843, 10.00000000000000000 ) ) ;
#8211 = DIRECTION ( 'NONE',  ( -1.000000000000000000, 0.000000000000000000, 0.000000000000000000 ) ) ;
#8212 = VERTEX_POINT ( 'NONE', #11440 ) ;
#8213 = DIRECTION ( 'NONE',  ( -1.000000000000000000, 0.000000000000000000, 0.000000000000000000 ) ) ;
#8214 = AXIS2_PLACEMENT_3D ( 'NONE', #8666, #4187, #265 ) ;
#8215 = ORIENTED_EDGE ( 'NONE', *, *, #288, .T. ) ;
#8216 = CARTESIAN_POINT ( 'NONE',  ( 5.657123057053811799, 5.504982807385217392, 3.747395293195558847E-16 ) ) ;
#8217 = LINE ( 'NONE', #10175, #1671 ) ;
#8218 = VERTEX_POINT ( 'NONE', #353 ) ;
#8219 = AXIS2_PLACEMENT_3D ( 'NONE', #11290, #11955, #7422 ) ;
#8220 = DIRECTION ( 'NONE',  ( -1.000000000000000000, 0.000000000000000000, 0.000000000000000000 ) ) ;
#8221 = VECTOR ( 'NONE', #2011, 1000.000000000000000 ) ;
#8222 = ADVANCED_FACE ( 'NONE', ( #9606 ), #1281, .T. ) ;
#8223 = AXIS2_PLACEMENT_3D ( 'NONE', #9439, #9375, #995 ) ;
#8224 = LINE ( 'NONE', #11949, #10385 ) ;
#8225 = DIRECTION ( 'NONE',  ( -1.000000000000000000, -0.000000000000000000, -0.000000000000000000 ) ) ;
#8226 = CARTESIAN_POINT ( 'NONE',  ( -8.739072045530903665, -14.04184524613901353, 10.00000000000000000 ) ) ;
#8228 = EDGE_CURVE ( 'NONE', #490, #110, #2314, .T. ) ;
#8227 = CARTESIAN_POINT ( 'NONE',  ( 4.764169229608189227, 7.652272242164855243, 6.857782953271941950E-17 ) ) ;
#8229 = DIRECTION ( 'NONE',  ( -1.000000000000000000, 0.000000000000000000, 0.000000000000000000 ) ) ;
#8230 = EDGE_CURVE ( 'NONE', #2524, #5042, #3502, .T. ) ;
#8231 = CARTESIAN_POINT ( 'NONE',  ( 0.000000000000000000, -22.21333432029571497, 11.02759168516737098 ) ) ;
#8232 = VERTEX_POINT ( 'NONE', #5875 ) ;
#8233 = AXIS2_PLACEMENT_3D ( 'NONE', #6380, #65, #1849 ) ;
#8234 = EDGE_LOOP ( 'NONE', ( #11605, #11617, #11403, #5745 ) ) ;
#8235 = CIRCLE ( 'NONE', #7841, 9.599999999999994316 ) ;
#8236 = ORIENTED_EDGE ( 'NONE', *, *, #9278, .F. ) ;
#8237 = VECTOR ( 'NONE', #3901, 1000.000000000000000 ) ;
#8238 = CARTESIAN_POINT ( 'NONE',  ( 12.96212312671954514, -3.473279994529783199, 10.00000000000000000 ) ) ;
#8239 = EDGE_CURVE ( 'NONE', #7393, #5404, #2720, .T. ) ;
#8240 = CARTESIAN_POINT ( 'NONE',  ( 0.000000000000000000, 17.31945870441147406, 15.13242714128125499 ) ) ;
#8241 = CARTESIAN_POINT ( 'NONE',  ( 3.000000000000000888, -20.41249101028218149, 9.589108953447823325 ) ) ;
#8242 = AXIS2_PLACEMENT_3D ( 'NONE', #11488, #4152, #6038 ) ;
#8243 = CARTESIAN_POINT ( 'NONE',  ( -3.663109177303993214, -5.348850660921103284, 3.747395293195558847E-16 ) ) ;
#8244 = DIRECTION ( 'NONE',  ( 0.000000000000000000, 0.000000000000000000, 1.000000000000000000 ) ) ;
#8245 = DIRECTION ( 'NONE',  ( 0.000000000000000000, 0.000000000000000000, 1.000000000000000000 ) ) ;
#8246 = VERTEX_POINT ( 'NONE', #1159 ) ;
#8247 = EDGE_CURVE ( 'NONE', #531, #10744, #4960, .T. ) ;
#8248 = VECTOR ( 'NONE', #1609, 1000.000000000000000 ) ;
#8249 = ORIENTED_EDGE ( 'NONE', *, *, #7263, .F. ) ;
#8250 = DIRECTION ( 'NONE',  ( -1.000000000000000000, -0.000000000000000000, -0.000000000000000000 ) ) ;
#8251 = AXIS2_PLACEMENT_3D ( 'NONE', #10144, #4278, #1703 ) ;
#8252 = EDGE_CURVE ( 'NONE', #8421, #8183, #6433, .T. ) ;
#8253 = LINE ( 'NONE', #10139, #573 ) ;
#8254 = EDGE_CURVE ( 'NONE', #9915, #10265, #964, .T. ) ;
#8255 = DIRECTION ( 'NONE',  ( -1.000000000000000000, 0.000000000000000000, 0.000000000000000000 ) ) ;
#8256 = DIRECTION ( 'NONE',  ( 0.000000000000000000, 0.000000000000000000, 1.000000000000000000 ) ) ;
#8257 = CARTESIAN_POINT ( 'NONE',  ( 3.000000000000000888, -1.901833551798412847, 22.47229024614976822 ) ) ;
#8258 = CARTESIAN_POINT ( 'NONE',  ( 8.235329212250112718, -1.783486464602660027, 6.857782953271941950E-17 ) ) ;
#8259 = AXIS2_PLACEMENT_3D ( 'NONE', #8257, #8993, #11804 ) ;
#8260 = FACE_OUTER_BOUND ( 'NONE', #8702, .T. ) ;
#8261 = CARTESIAN_POINT ( 'NONE',  ( 0.000000000000000000, 21.30300407174362576, -7.402892494506364329 ) ) ;
#8262 = ORIENTED_EDGE ( 'NONE', *, *, #8476, .F. ) ;
#8263 = EDGE_LOOP ( 'NONE', ( #8638, #6032, #3152, #10630 ) ) ;
#8264 = DIRECTION ( 'NONE',  ( -1.000000000000000000, 0.000000000000000000, -0.000000000000000000 ) ) ;
#8265 = ORIENTED_EDGE ( 'NONE', *, *, #3694, .T. ) ;
#8266 = ORIENTED_EDGE ( 'NONE', *, *, #6292, .F. ) ;
#8267 = CARTESIAN_POINT ( 'NONE',  ( 1.482756436301465808, -6.713508106970953015, 10.00000000000000000 ) ) ;
#8268 = EDGE_CURVE ( 'NONE', #6126, #5192, #8973, .T. ) ;
#8269 = ORIENTED_EDGE ( 'NONE', *, *, #11334, .F. ) ;
#8270 = DIRECTION ( 'NONE',  ( 0.000000000000000000, 0.000000000000000000, 1.000000000000000000 ) ) ;
#8271 = ORIENTED_EDGE ( 'NONE', *, *, #11033, .T. ) ;
#8272 = EDGE_LOOP ( 'NONE', ( #10399, #7764, #7687, #6617 ) ) ;
#8273 = CIRCLE ( 'NONE', #2407, 3.000000000000000444 ) ;
#8274 = CYLINDRICAL_SURFACE ( 'NONE', #10813, 9.599999999999997868 ) ;
#8275 = VECTOR ( 'NONE', #921, 1000.000000000000000 ) ;
#8276 = DIRECTION ( 'NONE',  ( -1.000000000000000000, 0.000000000000000000, -0.000000000000000000 ) ) ;
#8277 = CARTESIAN_POINT ( 'NONE',  ( -14.12277927129995803, -8.146689865454474599, 6.857782953271941950E-17 ) ) ;
#8278 = LINE ( 'NONE', #11875, #38 ) ;
#8279 = EDGE_CURVE ( 'NONE', #962, #7624, #4681, .T. ) ;
#8280 = CARTESIAN_POINT ( 'NONE',  ( 3.000000000000000888, 0.000000000000000000, 0.000000000000000000 ) ) ;
#8281 = CIRCLE ( 'NONE', #8489, 9.599999999999996092 ) ;
#8282 = CARTESIAN_POINT ( 'NONE',  ( 3.000000000000000888, 0.000000000000000000, 22.99899999999999878 ) ) ;
#8283 = ORIENTED_EDGE ( 'NONE', *, *, #1054, .F. ) ;
#8284 = CARTESIAN_POINT ( 'NONE',  ( 5.892341078160108658, -4.186101517074008349, 3.747395293195558847E-16 ) ) ;
#8285 = DIRECTION ( 'NONE',  ( 0.000000000000000000, -0.6691306063588495778, -0.7431448254774020157 ) ) ;
#8286 = CIRCLE ( 'NONE', #8495, 22.99899999999999878 ) ;
#8287 = DIRECTION ( 'NONE',  ( -0.000000000000000000, -0.000000000000000000, -1.000000000000000000 ) ) ;
#8288 = CARTESIAN_POINT ( 'NONE',  ( 3.000000000000000888, -7.432877647175053504, -21.76479567747249178 ) ) ;
#8289 = CARTESIAN_POINT ( 'NONE',  ( 0.000000000000000000, 14.74749645580011226, 17.06259499759949705 ) ) ;
#8290 = CYLINDRICAL_SURFACE ( 'NONE', #5709, 9.599999999999997868 ) ;
#8291 = CARTESIAN_POINT ( 'NONE',  ( 7.252227276001472767, 5.017415995114415495, 6.857782953271941950E-17 ) ) ;
#8292 = CARTESIAN_POINT ( 'NONE',  ( 3.000000000000000888, 6.168200451485758684, 24.02068490260614908 ) ) ;
#8293 = CARTESIAN_POINT ( 'NONE',  ( 0.000000000000000000, 0.000000000000000000, -15.00000000000000000 ) ) ;
#8294 = ORIENTED_EDGE ( 'NONE', *, *, #8074, .T. ) ;
#8295 = VERTEX_POINT ( 'NONE', #8987 ) ;
#8296 = AXIS2_PLACEMENT_3D ( 'NONE', #3084, #10244, #6745 ) ;
#8297 = VERTEX_POINT ( 'NONE', #12022 ) ;
#8298 = CARTESIAN_POINT ( 'NONE',  ( 3.000000000000000888, -22.99643626497956461, -0.3433949777334098785 ) ) ;
#8299 = CARTESIAN_POINT ( 'NONE',  ( 2.257301671556971367, -9.631158585656901749, 10.00000000000000000 ) ) ;
#8300 = ADVANCED_FACE ( 'NONE', ( #3705 ), #9904, .T. ) ;
#8301 = DIRECTION ( 'NONE',  ( 1.000000000000000000, 0.000000000000000000, 0.000000000000000000 ) ) ;
#8302 = DIRECTION ( 'NONE',  ( 0.000000000000000000, 0.7431448254773955764, -0.6691306063588569053 ) ) ;
#8303 = CARTESIAN_POINT ( 'NONE',  ( 4.889075487039526990, 9.929493272050624597, 3.747395293195558847E-16 ) ) ;
#8304 = AXIS2_PLACEMENT_3D ( 'NONE', #4473, #2700, #684 ) ;
#8305 = EDGE_CURVE ( 'NONE', #5168, #7882, #9756, .T. ) ;
#8306 = CARTESIAN_POINT ( 'NONE',  ( 0.8073695008816142993, 5.181225205791315958, 3.747395293195558847E-16 ) ) ;
#8307 = CYLINDRICAL_SURFACE ( 'NONE', #1583, 22.99899999999999878 ) ;
#8308 = ORIENTED_EDGE ( 'NONE', *, *, #10970, .F. ) ;
#8309 = ADVANCED_FACE ( 'NONE', ( #4273 ), #6457, .T. ) ;
#8310 = ORIENTED_EDGE ( 'NONE', *, *, #4108, .T. ) ;
#8311 = ORIENTED_EDGE ( 'NONE', *, *, #179, .T. ) ;
#8312 = EDGE_CURVE ( 'NONE', #10744, #7896, #7984, .T. ) ;
#8313 = ORIENTED_EDGE ( 'NONE', *, *, #9218, .F. ) ;
#8314 = DIRECTION ( 'NONE',  ( 0.000000000000000000, 0.000000000000000000, 1.000000000000000000 ) ) ;
#8315 = EDGE_CURVE ( 'NONE', #3911, #10594, #11798, .T. ) ;
#8316 = DIRECTION ( 'NONE',  ( 0.000000000000000000, -1.000000000000000000, -1.047444401652940007E-14 ) ) ;
#8317 = CARTESIAN_POINT ( 'NONE',  ( 3.000000000000000888, -22.56530478845645860, -4.445336973061090546 ) ) ;
#8318 = PRODUCT_DEFINITION_CONTEXT ( 'detailed design', #8009, 'design' ) ;
#8319 = DIRECTION ( 'NONE',  ( -1.000000000000000000, 0.000000000000000000, 0.000000000000000000 ) ) ;
#8320 = DIRECTION ( 'NONE',  ( -1.000000000000000000, 0.000000000000000000, 0.000000000000000000 ) ) ;
#8321 = CARTESIAN_POINT ( 'NONE',  ( -14.85975435031504510, 1.953672781916663936, 3.747395293195558847E-16 ) ) ;
#8322 = CARTESIAN_POINT ( 'NONE',  ( 2.919619825260425294, -7.400844473264723611, 6.857782953271941950E-17 ) ) ;
#8323 = CIRCLE ( 'NONE', #8119, 24.80000000000000071 ) ;
#8324 = CARTESIAN_POINT ( 'NONE',  ( 0.000000000000000000, -15.13242714128107913, -17.31945870441162683 ) ) ;
#8325 = DIRECTION ( 'NONE',  ( -1.000000000000000000, 0.000000000000000000, -0.000000000000000000 ) ) ;
#8326 = ORIENTED_EDGE ( 'NONE', *, *, #5924, .F. ) ;
#8327 = ORIENTED_EDGE ( 'NONE', *, *, #7310, .F. ) ;
#8328 = CARTESIAN_POINT ( 'NONE',  ( 0.000000000000000000, 0.000000000000000000, 0.000000000000000000 ) ) ;
#8329 = VERTEX_POINT ( 'NONE', #1808 ) ;
#8330 = CARTESIAN_POINT ( 'NONE',  ( -3.038216613430223756, 4.635879136410493651, 10.00000000000000000 ) ) ;
#8331 = VERTEX_POINT ( 'NONE', #5477 ) ;
#8332 = CYLINDRICAL_SURFACE ( 'NONE', #11068, 22.99899999999999878 ) ;
#8333 = VECTOR ( 'NONE', #9625, 1000.000000000000000 ) ;
#8334 = EDGE_LOOP ( 'NONE', ( #5631, #4876, #347, #4786 ) ) ;
#8335 = FACE_OUTER_BOUND ( 'NONE', #6060, .T. ) ;
#8336 = CARTESIAN_POINT ( 'NONE',  ( 3.000000000000000888, -9.039786367038701087, -21.14796121233205284 ) ) ;
#8337 = CARTESIAN_POINT ( 'NONE',  ( -6.191802569540381995, -3.848120238388911041, 10.00000000000000000 ) ) ;
#8338 = SURFACE_STYLE_USAGE ( .BOTH. , #927 ) ;
#8339 = ADVANCED_FACE ( 'NONE', ( #10886 ), #5547, .T. ) ;
#8340 = DIRECTION ( 'NONE',  ( 1.000000000000000000, 0.000000000000000000, 0.000000000000000000 ) ) ;
#8341 = ORIENTED_EDGE ( 'NONE', *, *, #5206, .F. ) ;
#8342 = CIRCLE ( 'NONE', #5602, 24.80000000000000071 ) ;
#8343 = VERTEX_POINT ( 'NONE', #9276 ) ;
#8344 = DIRECTION ( 'NONE',  ( 0.000000000000000000, 0.8660254037844398178, -0.4999999999999979461 ) ) ;
#8345 = ORIENTED_EDGE ( 'NONE', *, *, #218, .T. ) ;
#8346 = CARTESIAN_POINT ( 'NONE',  ( 1.482756436301464920, -6.713508106970949463, 3.747395293195558847E-16 ) ) ;
#8347 = DIRECTION ( 'NONE',  ( -1.000000000000000000, -1.445602896647338917E-16, 0.000000000000000000 ) ) ;
#8348 = FILL_AREA_STYLE ('',( #10176 ) ) ;
#8349 = EDGE_CURVE ( 'NONE', #4464, #11993, #4280, .T. ) ;
#8350 = CARTESIAN_POINT ( 'NONE',  ( 19.00000000000000000, 0.000000000000000000, -5.000000000000000000 ) ) ;
#8351 = LINE ( 'NONE', #10984, #5555 ) ;
#8352 = CARTESIAN_POINT ( 'NONE',  ( 3.000000000000000888, 19.75591328264900781, -10.87771529938142123 ) ) ;
#8353 = SHAPE_REPRESENTATION ( 'locker', ( #8474 ), #5098 ) ;
#8354 = CARTESIAN_POINT ( 'NONE',  ( 0.0002901587068756704066, -4.749354241797638210, 6.857782953271941950E-17 ) ) ;
#8355 =( NAMED_UNIT ( * ) SI_UNIT ( $, .STERADIAN. ) SOLID_ANGLE_UNIT ( ) );
#8356 = CARTESIAN_POINT ( 'NONE',  ( 0.000000000000000000, 0.000000000000000000, 20.00000000000000000 ) ) ;
#8357 = VERTEX_POINT ( 'NONE', #7135 ) ;
#8358 = ORIENTED_EDGE ( 'NONE', *, *, #998, .T. ) ;
#8359 = DIRECTION ( 'NONE',  ( -1.000000000000000000, -0.000000000000000000, -0.000000000000000000 ) ) ;
#8360 = CARTESIAN_POINT ( 'NONE',  ( 1.454091968623351550, 11.13059540125182778, 10.00000000000000000 ) ) ;
#8361 = CYLINDRICAL_SURFACE ( 'NONE', #6996, 22.99899999999999878 ) ;
#8362 = CARTESIAN_POINT ( 'NONE',  ( 0.000000000000000000, 8.645255683529009971, 23.24434456306328300 ) ) ;
#8363 = CARTESIAN_POINT ( 'NONE',  ( -9.037587479195730467, -0.7561632655184011842, 3.747395293195558847E-16 ) ) ;
#8364 = AXIS2_PLACEMENT_3D ( 'NONE', #5732, #3093, #11418 ) ;
#8365 = DIRECTION ( 'NONE',  ( 0.000000000000000000, 0.000000000000000000, 1.000000000000000000 ) ) ;
#8366 = VECTOR ( 'NONE', #2586, 1000.000000000000000 ) ;
#8367 = CARTESIAN_POINT ( 'NONE',  ( 3.000000000000000888, 20.78471918669860941, 8.753070780933226658 ) ) ;
#8368 = EDGE_LOOP ( 'NONE', ( #5814, #3667, #1348, #2077 ) ) ;
#8369 = VERTEX_POINT ( 'NONE', #10254 ) ;
#8370 = ORIENTED_EDGE ( 'NONE', *, *, #5338, .T. ) ;
#8371 = ORIENTED_EDGE ( 'NONE', *, *, #3143, .F. ) ;
#8372 = CARTESIAN_POINT ( 'NONE',  ( 3.000000000000000888, -16.45023496161675780, 15.42759117534379953 ) ) ;
#8373 = DIRECTION ( 'NONE',  ( 1.000000000000000000, 0.000000000000000000, -0.000000000000000000 ) ) ;
#8374 = VECTOR ( 'NONE', #10636, 1000.000000000000000 ) ;
#8375 = DIRECTION ( 'NONE',  ( 1.000000000000000000, 0.000000000000000000, 0.000000000000000000 ) ) ;
#8376 = CYLINDRICAL_SURFACE ( 'NONE', #9738, 9.599999999999997868 ) ;
#8377 = CIRCLE ( 'NONE', #6423, 9.599999999999997868 ) ;
#8378 = EDGE_CURVE ( 'NONE', #5811, #6304, #9334, .T. ) ;
#8379 = DIRECTION ( 'NONE',  ( -1.000000000000000000, -0.000000000000000000, 0.000000000000000000 ) ) ;
#8380 = EDGE_CURVE ( 'NONE', #10824, #1101, #11515, .T. ) ;
#8381 = CARTESIAN_POINT ( 'NONE',  ( 9.623054350189519823, -9.012277985855606133, 3.747395293195558847E-16 ) ) ;
#8382 = CARTESIAN_POINT ( 'NONE',  ( -4.263796145714473518, -6.152586724582786104, 6.857782953271941950E-17 ) ) ;
#8383 = EDGE_CURVE ( 'NONE', #6456, #622, #173, .T. ) ;
#8384 = CARTESIAN_POINT ( 'NONE',  ( 3.000000000000000888, 1.901833551798254973, 22.47229024614977888 ) ) ;
#8385 = AXIS2_PLACEMENT_3D ( 'NONE', #7888, #476, #8873 ) ;
#8386 = ORIENTED_EDGE ( 'NONE', *, *, #3518, .T. ) ;
#8387 = ORIENTED_EDGE ( 'NONE', *, *, #7114, .F. ) ;
#8388 = CYLINDRICAL_SURFACE ( 'NONE', #2358, 24.80000000000000071 ) ;
#8389 = VERTEX_POINT ( 'NONE', #6116 ) ;
#8390 = FACE_OUTER_BOUND ( 'NONE', #7494, .T. ) ;
#8391 = CARTESIAN_POINT ( 'NONE',  ( 0.000000000000000000, 9.667200211210106531, -20.86861857134724474 ) ) ;
#8392 = ORIENTED_EDGE ( 'NONE', *, *, #8754, .F. ) ;
#8393 = ADVANCED_FACE ( 'NONE', ( #6235, #11737 ), #1741, .F. ) ;
#8394 = AXIS2_PLACEMENT_3D ( 'NONE', #9544, #6838, #1224 ) ;
#8395 = DIRECTION ( 'NONE',  ( -1.000000000000000000, 8.673617379884035472E-16, 0.000000000000000000 ) ) ;
#8396 = DIRECTION ( 'NONE',  ( -1.000000000000000000, 0.000000000000000000, 0.000000000000000000 ) ) ;
#8397 = CARTESIAN_POINT ( 'NONE',  ( -8.739072045530900112, -14.04184524613900820, 6.857782953271941950E-17 ) ) ;
#8398 = DIRECTION ( 'NONE',  ( -1.000000000000000000, 0.000000000000000000, 0.000000000000000000 ) ) ;
#8399 = CARTESIAN_POINT ( 'NONE',  ( 3.000000000000000888, 0.000000000000000000, 0.000000000000000000 ) ) ;
#8400 = CARTESIAN_POINT ( 'NONE',  ( 0.000000000000000000, 0.000000000000000000, 0.000000000000000000 ) ) ;
#8401 = DIRECTION ( 'NONE',  ( -1.000000000000000000, 0.000000000000000000, 0.000000000000000000 ) ) ;
#8402 = ORIENTED_EDGE ( 'NONE', *, *, #5843, .T. ) ;
#8403 = AXIS2_PLACEMENT_3D ( 'NONE', #1282, #5015, #8751 ) ;
#8404 = CIRCLE ( 'NONE', #6823, 22.99900000000000233 ) ;
#8405 = EDGE_CURVE ( 'NONE', #246, #8841, #2439, .T. ) ;
#8406 = CARTESIAN_POINT ( 'NONE',  ( -11.99326810842507562, 8.590522060507204571, 10.00000000000000000 ) ) ;
#8407 = AXIS2_PLACEMENT_3D ( 'NONE', #10936, #10134, #1986 ) ;
#8408 = LINE ( 'NONE', #5718, #4620 ) ;
#8409 = EDGE_CURVE ( 'NONE', #10512, #5151, #7034, .T. ) ;
#8410 = DIRECTION ( 'NONE',  ( -1.000000000000000000, -0.000000000000000000, 0.000000000000000000 ) ) ;
#8411 = CARTESIAN_POINT ( 'NONE',  ( 3.000000000000000888, -5.117118920208643118, 22.42251312757878168 ) ) ;
#8412 = CARTESIAN_POINT ( 'NONE',  ( -7.575117642440520882, -14.74712341115847103, 10.00000000000000000 ) ) ;
#8413 = AXIS2_PLACEMENT_3D ( 'NONE', #3164, #5796, #2059 ) ;
#8414 = CARTESIAN_POINT ( 'NONE',  ( 5.247589697392725405, -6.187652788349031319, 6.857782953271941950E-17 ) ) ;
#8415 = CARTESIAN_POINT ( 'NONE',  ( 0.000000000000000000, 22.83456483164692941, -2.745295967525760439 ) ) ;
#8416 = CIRCLE ( 'NONE', #6831, 9.599999999999997868 ) ;
#8417 = DIRECTION ( 'NONE',  ( 0.000000000000000000, 0.000000000000000000, 1.000000000000000000 ) ) ;
#8418 = ORIENTED_EDGE ( 'NONE', *, *, #2396, .T. ) ;
#8419 = EDGE_CURVE ( 'NONE', #429, #7212, #8787, .T. ) ;
#8420 =( REPRESENTATION_RELATIONSHIP ('NONE','NONE', #8743, #6315 ) REPRESENTATION_RELATIONSHIP_WITH_TRANSFORMATION ( #661 )SHAPE_REPRESENTATION_RELATIONSHIP( ) );
#8421 = VERTEX_POINT ( 'NONE', #2395 ) ;
#8422 = EDGE_LOOP ( 'NONE', ( #11439, #6005, #10628, #4170 ) ) ;
#8423 = AXIS2_PLACEMENT_3D ( 'NONE', #321, #4123, #11590 ) ;
#8424 = DIRECTION ( 'NONE',  ( -1.000000000000000000, -0.000000000000000000, -0.000000000000000000 ) ) ;
#8425 = AXIS2_PLACEMENT_3D ( 'NONE', #6061, #8010, #7897 ) ;
#8426 = CARTESIAN_POINT ( 'NONE',  ( -8.409270314015810044, 2.833341551407463133, 10.00000000000000000 ) ) ;
#8427 = CIRCLE ( 'NONE', #1573, 9.599999999999997868 ) ;
#8428 = CARTESIAN_POINT ( 'NONE',  ( 3.000000000000000888, 15.80756504416717334, -19.10918332567941746 ) ) ;
#8429 = DIRECTION ( 'NONE',  ( -1.000000000000000000, 0.000000000000000000, 0.000000000000000000 ) ) ;
#8430 = MANIFOLD_SOLID_BREP ( 'Extrude-Thin1', #4529 ) ;
#8431 = CARTESIAN_POINT ( 'NONE',  ( -4.046710180314748939, 10.72208681399755292, 3.747395293195558847E-16 ) ) ;
#8432 = CARTESIAN_POINT ( 'NONE',  ( 0.000000000000000000, -20.08719549084857192, -11.20082935824096459 ) ) ;
#8433 = AXIS2_PLACEMENT_3D ( 'NONE', #991, #5402, #4548 ) ;
#8434 = DIRECTION ( 'NONE',  ( -1.000000000000000000, 0.000000000000000000, 0.000000000000000000 ) ) ;
#8435 = CIRCLE ( 'NONE', #4520, 9.600000000000001421 ) ;
#8436 = ORIENTED_EDGE ( 'NONE', *, *, #5368, .T. ) ;
#8437 = ADVANCED_FACE ( 'NONE', ( #909 ), #5563, .T. ) ;
#8438 = EDGE_CURVE ( 'NONE', #2943, #6856, #7400, .T. ) ;
#8439 = AXIS2_PLACEMENT_3D ( 'NONE', #8328, #3554, #11021 ) ;
#8440 = EDGE_LOOP ( 'NONE', ( #747, #9046, #676, #5146 ) ) ;
#8441 = EDGE_LOOP ( 'NONE', ( #10909, #4602, #1655, #7620 ) ) ;
#8442 = CARTESIAN_POINT ( 'NONE',  ( 0.000000000000000000, -22.42251312757876036, -5.117118920208720390 ) ) ;
#8443 = CARTESIAN_POINT ( 'NONE',  ( 0.000000000000000000, 3.623565124517433400, -24.53384959170453783 ) ) ;
#8444 = VECTOR ( 'NONE', #11715, 1000.000000000000000 ) ;
#8445 = DIRECTION ( 'NONE',  ( -1.000000000000000000, 0.000000000000000000, 0.000000000000000000 ) ) ;
#8446 = PLANE ( 'NONE',  #6993 ) ;
#8447 = CIRCLE ( 'NONE', #7642, 22.99899999999999523 ) ;
#8448 = DIRECTION ( 'NONE',  ( 0.000000000000000000, 0.000000000000000000, -1.000000000000000000 ) ) ;
#8449 = CARTESIAN_POINT ( 'NONE',  ( 7.081399987883180813, -10.98142027556026612, 3.747395293195558847E-16 ) ) ;
#8450 =( NAMED_UNIT ( * ) PLANE_ANGLE_UNIT ( ) SI_UNIT ( $, .RADIAN. ) );
#8451 = AXIS2_PLACEMENT_3D ( 'NONE', #1122, #3879, #2100 ) ;
#8452 = DIRECTION ( 'NONE',  ( -1.000000000000000000, -0.000000000000000000, -0.000000000000000000 ) ) ;
#8453 = ORIENTED_EDGE ( 'NONE', *, *, #9789, .T. ) ;
#8454 = ORIENTED_EDGE ( 'NONE', *, *, #2993, .F. ) ;
#8455 = CARTESIAN_POINT ( 'NONE',  ( 0.000000000000000000, 0.000000000000000000, 0.000000000000000000 ) ) ;
#8456 = CIRCLE ( 'NONE', #3173, 9.599999999999996092 ) ;
#8457 = EDGE_LOOP ( 'NONE', ( #8326, #7327, #1952, #2577 ) ) ;
#8458 = VERTEX_POINT ( 'NONE', #8317 ) ;
#8459 = DIRECTION ( 'NONE',  ( 1.000000000000000000, 0.000000000000000000, 0.000000000000000000 ) ) ;
#8460 = DIRECTION ( 'NONE',  ( 0.000000000000000000, 0.000000000000000000, 1.000000000000000000 ) ) ;
#8461 = ORIENTED_EDGE ( 'NONE', *, *, #8616, .F. ) ;
#8462 = EDGE_CURVE ( 'NONE', #6967, #3076, #8087, .T. ) ;
#8463 = AXIS2_PLACEMENT_3D ( 'NONE', #1166, #1393, #11393 ) ;
#8464 = CIRCLE ( 'NONE', #4543, 9.599999999999997868 ) ;
#8465 = CARTESIAN_POINT ( 'NONE',  ( 3.000000000000000888, 0.000000000000000000, 0.000000000000000000 ) ) ;
#8466 = LINE ( 'NONE', #925, #10602 ) ;
#8467 = CARTESIAN_POINT ( 'NONE',  ( 7.014224211608840243, -15.49593329755746218, 6.857782953271941950E-17 ) ) ;
#8468 = DIRECTION ( 'NONE',  ( -0.07332096784668425127, -0.9973083954695386444, 0.000000000000000000 ) ) ;
#8469 = DIRECTION ( 'NONE',  ( 0.000000000000000000, -0.5877852522924630341, -0.8090169943749546677 ) ) ;
#8470 = ORIENTED_EDGE ( 'NONE', *, *, #771, .F. ) ;
#8471 = CARTESIAN_POINT ( 'NONE',  ( 1.500000000000000444, -19.43515443678412780, 15.40502424595139530 ) ) ;
#8472 = ORIENTED_EDGE ( 'NONE', *, *, #1342, .F. ) ;
#8473 = EDGE_CURVE ( 'NONE', #11218, #3365, #3700, .T. ) ;
#8474 = AXIS2_PLACEMENT_3D ( 'NONE', #1674, #1551, #2653 ) ;
#8475 = CARTESIAN_POINT ( 'NONE',  ( -14.85975435031504865, 1.953672781916663936, 10.00000000000000000 ) ) ;
#8476 = EDGE_CURVE ( 'NONE', #11323, #12055, #8598, .T. ) ;
#8477 = AXIS2_PLACEMENT_3D ( 'NONE', #11589, #7729, #8838 ) ;
#8478 = CYLINDRICAL_SURFACE ( 'NONE', #1095, 9.599999999999996092 ) ;
#8479 = DIRECTION ( 'NONE',  ( -0.000000000000000000, -0.000000000000000000, 1.000000000000000000 ) ) ;
#8480 = DIRECTION ( 'NONE',  ( 1.000000000000000000, -0.000000000000000000, 0.000000000000000000 ) ) ;
#8481 = CARTESIAN_POINT ( 'NONE',  ( -15.56595607421884075, -4.438723023272252988, 10.00000000000000000 ) ) ;
#8482 = AXIS2_PLACEMENT_3D ( 'NONE', #10228, #7646, #4780 ) ;
#8483 = CARTESIAN_POINT ( 'NONE',  ( -5.152979166089614260, -5.321787192520350374, 6.857782953271941950E-17 ) ) ;
#8484 = CYLINDRICAL_SURFACE ( 'NONE', #1760, 9.599999999999997868 ) ;
#8485 = AXIS2_PLACEMENT_3D ( 'NONE', #6839, #4274, #10701 ) ;
#8486 = VERTEX_POINT ( 'NONE', #3380 ) ;
#8487 = FACE_OUTER_BOUND ( 'NONE', #7009, .T. ) ;
#8488 = ORIENTED_EDGE ( 'NONE', *, *, #6499, .F. ) ;
#8489 = AXIS2_PLACEMENT_3D ( 'NONE', #10891, #5199, #11016 ) ;
#8490 = DIRECTION ( 'NONE',  ( 0.000000000000000000, 0.000000000000000000, 1.000000000000000000 ) ) ;
#8491 = CARTESIAN_POINT ( 'NONE',  ( 4.583115687978493114, -8.898851689027766909, 10.00000000000000000 ) ) ;
#8492 = DIRECTION ( 'NONE',  ( 1.000000000000000000, -0.000000000000000000, -0.000000000000000000 ) ) ;
#8493 = CARTESIAN_POINT ( 'NONE',  ( -1.515734900794040385, 8.225284064336934264, 3.747395293195558847E-16 ) ) ;
#8494 = DIRECTION ( 'NONE',  ( 1.000000000000000000, -0.000000000000000000, -0.000000000000000000 ) ) ;
#8495 = AXIS2_PLACEMENT_3D ( 'NONE', #9934, #2992, #10451 ) ;
#8496 = CARTESIAN_POINT ( 'NONE',  ( 3.000000000000000888, 13.23915371906955052, 18.80635025205174671 ) ) ;
#8497 = ORIENTED_EDGE ( 'NONE', *, *, #5552, .F. ) ;
#8498 = EDGE_CURVE ( 'NONE', #10826, #10797, #10534, .T. ) ;
#8499 = ADVANCED_BREP_SHAPE_REPRESENTATION ( '', ( #8710, #8474 ), #4902 ) ;
#8500 = VERTEX_POINT ( 'NONE', #6194 ) ;
#8501 = ORIENTED_EDGE ( 'NONE', *, *, #5312, .T. ) ;
#8502 = LINE ( 'NONE', #7621, #59 ) ;
#8503 = CARTESIAN_POINT ( 'NONE',  ( 1.500000000000000444, -23.05871956130128808, 9.128825345752947129 ) ) ;
#8504 = CIRCLE ( 'NONE', #9273, 22.99900000000000233 ) ;
#8505 = DIRECTION ( 'NONE',  ( 0.000000000000000000, 0.000000000000000000, 1.000000000000000000 ) ) ;
#8506 = CARTESIAN_POINT ( 'NONE',  ( 3.000000000000000888, 0.000000000000000000, 0.000000000000000000 ) ) ;
#8507 = EDGE_CURVE ( 'NONE', #5406, #10107, #1534, .T. ) ;
#8508 = DIRECTION ( 'NONE',  ( 0.000000000000000000, 0.000000000000000000, 1.000000000000000000 ) ) ;
#8509 = CARTESIAN_POINT ( 'NONE',  ( 4.163410377374355598, -12.26152398776834040, 3.747395293195558847E-16 ) ) ;
#8510 = DIRECTION ( 'NONE',  ( -0.000000000000000000, -0.000000000000000000, -1.000000000000000000 ) ) ;
#8511 = VERTEX_POINT ( 'NONE', #11979 ) ;
#8512 = VERTEX_POINT ( 'NONE', #3608 ) ;
#8513 = CARTESIAN_POINT ( 'NONE',  ( -15.59049818040342927, 3.373450308083567606, 10.00000000000000000 ) ) ;
#8514 = EDGE_LOOP ( 'NONE', ( #4696, #8141, #9970, #8527 ) ) ;
#8515 = DIRECTION ( 'NONE',  ( -1.000000000000000000, -0.000000000000000000, -0.000000000000000000 ) ) ;
#8516 = DIRECTION ( 'NONE',  ( 1.000000000000000000, 0.000000000000000000, 0.000000000000000000 ) ) ;
#8517 = VERTEX_POINT ( 'NONE', #6414 ) ;
#8518 = DIRECTION ( 'NONE',  ( -1.000000000000000000, 0.000000000000000000, 0.000000000000000000 ) ) ;
#8519 = AXIS2_PLACEMENT_3D ( 'NONE', #9818, #5165, #3327 ) ;
#8520 = CARTESIAN_POINT ( 'NONE',  ( 3.000000000000000888, 16.45023496161686438, -15.42759117534368407 ) ) ;
#8521 = CARTESIAN_POINT ( 'NONE',  ( -12.72059027619867244, -3.407653011835690471, 6.857782953271941950E-17 ) ) ;
#8522 = LINE ( 'NONE', #5126, #3371 ) ;
#8523 = DIRECTION ( 'NONE',  ( 0.000000000000000000, 0.000000000000000000, 1.000000000000000000 ) ) ;
#8524 = ORIENTED_EDGE ( 'NONE', *, *, #5798, .T. ) ;
#8525 = ORIENTED_EDGE ( 'NONE', *, *, #1092, .F. ) ;
#8526 = DIRECTION ( 'NONE',  ( 0.000000000000000000, 0.000000000000000000, 1.000000000000000000 ) ) ;
#8527 = ORIENTED_EDGE ( 'NONE', *, *, #8473, .T. ) ;
#8528 = AXIS2_PLACEMENT_3D ( 'NONE', #10962, #2640, #10158 ) ;
#8529 = CARTESIAN_POINT ( 'NONE',  ( 15.52845182490561626, -5.270724383582042982, 10.00000000000000000 ) ) ;
#8530 = EDGE_CURVE ( 'NONE', #4684, #2848, #5260, .T. ) ;
#8531 = DIRECTION ( 'NONE',  ( -0.000000000000000000, -0.000000000000000000, -1.000000000000000000 ) ) ;
#8532 = DIRECTION ( 'NONE',  ( -1.000000000000000000, 0.000000000000000000, 0.000000000000000000 ) ) ;
#8533 = CYLINDRICAL_SURFACE ( 'NONE', #673, 9.599999999999997868 ) ;
#8534 = CARTESIAN_POINT ( 'NONE',  ( 13.92981926110968161, -3.738495919395732781, 10.00000000000000000 ) ) ;
#8535 = PRODUCT_RELATED_PRODUCT_CATEGORY ( 'part', '', ( #9411 ) ) ;
#8536 = AXIS2_PLACEMENT_3D ( 'NONE', #8701, #10649, #3122 ) ;
#8537 = CARTESIAN_POINT ( 'NONE',  ( 3.000000000000000888, 11.67026512804572924, -19.29833442572348190 ) ) ;
#8538 = DIRECTION ( 'NONE',  ( 0.000000000000000000, 0.8660254037844363761, 0.5000000000000039968 ) ) ;
#8539 = EDGE_CURVE ( 'NONE', #5263, #505, #7204, .T. ) ;
#8540 = CARTESIAN_POINT ( 'NONE',  ( 3.000000000000000888, -16.85990652506889376, -15.64281154287614584 ) ) ;
#8541 = VERTEX_POINT ( 'NONE', #6473 ) ;
#8542 = EDGE_CURVE ( 'NONE', #8125, #10492, #4482, .T. ) ;
#8543 = CARTESIAN_POINT ( 'NONE',  ( -10.00000000000000000, 0.000000000000000000, 0.000000000000000000 ) ) ;
#8544 = ORIENTED_EDGE ( 'NONE', *, *, #11382, .F. ) ;
#8545 = AXIS2_PLACEMENT_3D ( 'NONE', #11740, #8002, #4522 ) ;
#8546 = FACE_BOUND ( 'NONE', #11852, .T. ) ;
#8547 = CARTESIAN_POINT ( 'NONE',  ( -7.812220363924760491, -5.053636123081433951, 10.00000000000000000 ) ) ;
#8548 = CARTESIAN_POINT ( 'NONE',  ( 3.000000000000000888, 22.54798042742718067, -0.4575788569252652871 ) ) ;
#8549 = CARTESIAN_POINT ( 'NONE',  ( -2.196651480121880162, 8.111327970581170277, 3.747395293195558847E-16 ) ) ;
#8550 = CARTESIAN_POINT ( 'NONE',  ( 13.14573027368987646, 6.745762002080606834, 6.857782953271941950E-17 ) ) ;
#8551 = DIRECTION ( 'NONE',  ( -1.000000000000000000, 0.000000000000000000, 0.000000000000000000 ) ) ;
#8552 = ORIENTED_EDGE ( 'NONE', *, *, #4492, .T. ) ;
#8553 = ORIENTED_EDGE ( 'NONE', *, *, #4533, .F. ) ;
#8554 = ORIENTED_EDGE ( 'NONE', *, *, #10555, .T. ) ;
#8555 = CARTESIAN_POINT ( 'NONE',  ( 3.000000000000000888, 0.000000000000000000, 0.000000000000000000 ) ) ;
#8556 = EDGE_CURVE ( 'NONE', #900, #2329, #6648, .T. ) ;
#8557 = DIRECTION ( 'NONE',  ( -1.000000000000000000, 0.000000000000000000, -0.000000000000000000 ) ) ;
#8558 = DIRECTION ( 'NONE',  ( 1.000000000000000000, 0.000000000000000000, 0.000000000000000000 ) ) ;
#8559 = DIRECTION ( 'NONE',  ( -1.000000000000000000, 0.000000000000000000, 0.000000000000000000 ) ) ;
#8560 = EDGE_CURVE ( 'NONE', #1454, #8857, #11324, .T. ) ;
#8561 = AXIS2_PLACEMENT_3D ( 'NONE', #4489, #8220, #2654 ) ;
#8562 = DIRECTION ( 'NONE',  ( 1.000000000000000000, 0.000000000000000000, 0.000000000000000000 ) ) ;
#8563 = CARTESIAN_POINT ( 'NONE',  ( 3.885483365683944257, 13.62125166200964976, 3.747395293195558847E-16 ) ) ;
#8564 = EDGE_CURVE ( 'NONE', #7059, #2212, #765, .T. ) ;
#8565 = DIRECTION ( 'NONE',  ( -1.000000000000000000, -0.000000000000000000, 0.000000000000000000 ) ) ;
#8566 = VERTEX_POINT ( 'NONE', #3847 ) ;
#8567 = ORIENTED_EDGE ( 'NONE', *, *, #148, .T. ) ;
#8568 = DIRECTION ( 'NONE',  ( 0.000000000000000000, 1.000000000000000000, 0.000000000000000000 ) ) ;
#8569 = CARTESIAN_POINT ( 'NONE',  ( 16.47843063274657993, -5.593696103119286001, 10.00000000000000000 ) ) ;
#8570 = ADVANCED_FACE ( 'NONE', ( #5750 ), #6590, .T. ) ;
#8571 = EDGE_LOOP ( 'NONE', ( #5117, #310, #8753, #11647 ) ) ;
#8572 = AXIS2_PLACEMENT_3D ( 'NONE', #4386, #4442, #8118 ) ;
#8573 = CARTESIAN_POINT ( 'NONE',  ( 0.000000000000000000, -11.02759168516760013, 22.21333432029560129 ) ) ;
#8574 = CYLINDRICAL_SURFACE ( 'NONE', #11465, 22.99899999999999878 ) ;
#8575 = ORIENTED_EDGE ( 'NONE', *, *, #8507, .T. ) ;
#8576 = DIRECTION ( 'NONE',  ( 0.000000000000000000, 0.2079116908177597312, -0.9781476007338056888 ) ) ;
#8577 = DIRECTION ( 'NONE',  ( 0.000000000000000000, 0.000000000000000000, 1.000000000000000000 ) ) ;
#8578 = CARTESIAN_POINT ( 'NONE',  ( -6.266017822847494756, 10.86399168115690728, 6.857782953271941950E-17 ) ) ;
#8579 = VECTOR ( 'NONE', #5751, 1000.000000000000000 ) ;
#8580 = AXIS2_PLACEMENT_3D ( 'NONE', #12084, #4441, #652 ) ;
#8581 = LINE ( 'NONE', #9770, #7640 ) ;
#8582 = EDGE_CURVE ( 'NONE', #2749, #5671, #6250, .T. ) ;
#8583 = LINE ( 'NONE', #9676, #1606 ) ;
#8584 = EDGE_LOOP ( 'NONE', ( #2957, #1338, #11541, #10462 ) ) ;
#8585 = ORIENTED_EDGE ( 'NONE', *, *, #7139, .F. ) ;
#8586 = FACE_OUTER_BOUND ( 'NONE', #10382, .T. ) ;
#8587 = ORIENTED_EDGE ( 'NONE', *, *, #2946, .F. ) ;
#8588 = CARTESIAN_POINT ( 'NONE',  ( -13.25288834650809910, -7.646628085889272342, 10.00000000000000000 ) ) ;
#8589 = AXIS2_PLACEMENT_3D ( 'NONE', #1506, #5423, #4506 ) ;
#8590 = CYLINDRICAL_SURFACE ( 'NONE', #10283, 22.00000000000000000 ) ;
#8591 = CARTESIAN_POINT ( 'NONE',  ( 13.67726327739689829, -10.50289975150003485, 6.857782953271941950E-17 ) ) ;
#8592 = CARTESIAN_POINT ( 'NONE',  ( 1.500000000000000444, 17.35216073792440739, 17.71842311621535870 ) ) ;
#8593 = CARTESIAN_POINT ( 'NONE',  ( 3.000000000000000888, 0.000000000000000000, 0.000000000000000000 ) ) ;
#8594 = CARTESIAN_POINT ( 'NONE',  ( 2.578468386369561216, 11.91291369680097567, 10.00000000000000000 ) ) ;
#8595 = DIRECTION ( 'NONE',  ( -1.000000000000000000, -0.000000000000000000, 0.000000000000000000 ) ) ;
#8596 = LINE ( 'NONE', #10541, #5342 ) ;
#8597 = AXIS2_PLACEMENT_3D ( 'NONE', #2440, #7315, #6236 ) ;
#8598 = CIRCLE ( 'NONE', #3308, 24.80000000000000071 ) ;
#8599 = DIRECTION ( 'NONE',  ( -1.000000000000000000, -0.000000000000000000, 0.000000000000000000 ) ) ;
#8600 = CARTESIAN_POINT ( 'NONE',  ( 1.499999999999999556, 23.05871956130122413, 9.128825345753105225 ) ) ;
#8601 = EDGE_LOOP ( 'NONE', ( #6328, #2510, #4381, #10832 ) ) ;
#8602 = ORIENTED_EDGE ( 'NONE', *, *, #2825, .T. ) ;
#8603 = AXIS2_PLACEMENT_3D ( 'NONE', #7735, #11473, #5907 ) ;
#8604 = CARTESIAN_POINT ( 'NONE',  ( -19.00000000000000000, 2.326828918379970970E-15, -5.000000000000000000 ) ) ;
#8605 = CARTESIAN_POINT ( 'NONE',  ( 3.120778274233608318, -6.257845451232916467, 10.00000000000000000 ) ) ;
#8606 = EDGE_CURVE ( 'NONE', #843, #10512, #5267, .T. ) ;
#8607 = CARTESIAN_POINT ( 'NONE',  ( -10.00000000000000000, 0.000000000000000000, 0.000000000000000000 ) ) ;
#8608 = ADVANCED_FACE ( 'NONE', ( #10325 ), #1944, .T. ) ;
#8609 = CIRCLE ( 'NONE', #1566, 9.599999999999997868 ) ;
#8610 = CARTESIAN_POINT ( 'NONE',  ( 5.027256439335601179, -9.798587832406491671, 10.00000000000000000 ) ) ;
#8611 = CARTESIAN_POINT ( 'NONE',  ( -15.56595607421883365, -4.438723023272252100, 6.857782953271941950E-17 ) ) ;
#8612 = FACE_OUTER_BOUND ( 'NONE', #5771, .T. ) ;
#8613 = VERTEX_POINT ( 'NONE', #2868 ) ;
#8614 = VECTOR ( 'NONE', #3020, 1000.000000000000000 ) ;
#8615 = ORIENTED_EDGE ( 'NONE', *, *, #7814, .T. ) ;
#8616 = EDGE_CURVE ( 'NONE', #11379, #8825, #8404, .T. ) ;
#8617 = CYLINDRICAL_SURFACE ( 'NONE', #2295, 24.80000000000000071 ) ;
#8618 = DIRECTION ( 'NONE',  ( 1.000000000000000000, 0.000000000000000000, 0.000000000000000000 ) ) ;
#8619 = ADVANCED_FACE ( 'NONE', ( #2121 ), #1212, .T. ) ;
#8620 = EDGE_LOOP ( 'NONE', ( #11824, #3341 ) ) ;
#8621 = CARTESIAN_POINT ( 'NONE',  ( 3.000000000000000888, 0.000000000000000000, 0.000000000000000000 ) ) ;
#8622 = CARTESIAN_POINT ( 'NONE',  ( 1.499999999999999556, 23.05871956130134492, -9.128825345752797915 ) ) ;
#8623 = CARTESIAN_POINT ( 'NONE',  ( 22.00000000000000000, 2.694222958124176809E-15, 3.000000000000000000 ) ) ;
#8624 = VECTOR ( 'NONE', #11205, 1000.000000000000000 ) ;
#8625 = CARTESIAN_POINT ( 'NONE',  ( -11.92955594661033203, -2.174140050202131302, 3.747395293195558847E-16 ) ) ;
#8626 = EDGE_CURVE ( 'NONE', #8200, #10186, #4949, .T. ) ;
#8627 = CYLINDRICAL_SURFACE ( 'NONE', #1356, 22.99899999999999878 ) ;
#8628 = ORIENTED_EDGE ( 'NONE', *, *, #11223, .F. ) ;
#8629 = VERTEX_POINT ( 'NONE', #7567 ) ;
#8630 = CARTESIAN_POINT ( 'NONE',  ( -14.12277927129996158, -8.146689865454478152, 10.00000000000000000 ) ) ;
#8631 = ORIENTED_EDGE ( 'NONE', *, *, #5449, .F. ) ;
#8632 = AXIS2_PLACEMENT_3D ( 'NONE', #5768, #9491, #178 ) ;
#8633 = ADVANCED_FACE ( 'NONE', ( #2186 ), #11309, .T. ) ;
#8634 = DIRECTION ( 'NONE',  ( -1.000000000000000000, 0.000000000000000000, -0.000000000000000000 ) ) ;
#8635 = DIRECTION ( 'NONE',  ( 1.000000000000000000, 0.000000000000000000, -0.000000000000000000 ) ) ;
#8636 = CIRCLE ( 'NONE', #1403, 9.599999999999996092 ) ;
#8637 = CARTESIAN_POINT ( 'NONE',  ( 1.500000000000000222, 0.000000000000000000, 4.000000000000000000 ) ) ;
#8638 = ORIENTED_EDGE ( 'NONE', *, *, #3898, .F. ) ;
#8639 = DIRECTION ( 'NONE',  ( 0.000000000000000000, 0.000000000000000000, 1.000000000000000000 ) ) ;
#8640 = CARTESIAN_POINT ( 'NONE',  ( 3.000000000000000888, 0.000000000000000000, 0.000000000000000000 ) ) ;
#8641 = CARTESIAN_POINT ( 'NONE',  ( 8.588976300537435549, -11.19439025337200810, 6.857782953271941950E-17 ) ) ;
#8642 = PRODUCT ( 'spring holder_ISO - Spur gear 0.8M 60T 20PA 3FW ---S60A75H50L8.0N', 'spring holder_ISO - Spur gear 0.8M 60T 20PA 3FW ---S60A75H50L8.0N', '', ( #10016 ) ) ;
#8643 = DIRECTION ( 'NONE',  ( 0.000000000000000000, 0.000000000000000000, 1.000000000000000000 ) ) ;
#8644 = ORIENTED_EDGE ( 'NONE', *, *, #10053, .F. ) ;
#8645 = CIRCLE ( 'NONE', #7058, 9.599999999999997868 ) ;
#8646 = FACE_OUTER_BOUND ( 'NONE', #10235, .T. ) ;
#8647 = VERTEX_POINT ( 'NONE', #3903 ) ;
#8648 = CARTESIAN_POINT ( 'NONE',  ( 0.000000000000000000, 0.000000000000000000, 0.000000000000000000 ) ) ;
#8649 = ORIENTED_EDGE ( 'NONE', *, *, #2927, .T. ) ;
#8650 = EDGE_CURVE ( 'NONE', #2737, #6263, #574, .T. ) ;
#8651 = CARTESIAN_POINT ( 'NONE',  ( -8.207979594962568015, -13.19054478262514607, 10.00000000000000000 ) ) ;
#8652 =( GEOMETRIC_REPRESENTATION_CONTEXT ( 3 ) GLOBAL_UNCERTAINTY_ASSIGNED_CONTEXT ( ( #5500 ) ) GLOBAL_UNIT_ASSIGNED_CONTEXT ( ( #2591, #5582, #10102 ) ) REPRESENTATION_CONTEXT ( 'NONE', 'WORKASPACE' ) );
#8653 = CIRCLE ( 'NONE', #10398, 24.80000000000000071 ) ;
#8654 = DIRECTION ( 'NONE',  ( -1.000000000000000000, 0.000000000000000000, 0.000000000000000000 ) ) ;
#8655 = ORIENTED_EDGE ( 'NONE', *, *, #1429, .T. ) ;
#8656 =( REPRESENTATION_RELATIONSHIP ('NONE','NONE', #8743, #7555 ) REPRESENTATION_RELATIONSHIP_WITH_TRANSFORMATION ( #7252 )SHAPE_REPRESENTATION_RELATIONSHIP( ) );
#8657 = DIRECTION ( 'NONE',  ( -1.000000000000000000, 0.000000000000000000, 0.000000000000000000 ) ) ;
#8658 = EDGE_CURVE ( 'NONE', #6529, #8051, #7412, .T. ) ;
#8659 = DIRECTION ( 'NONE',  ( -0.000000000000000000, -0.000000000000000000, -1.000000000000000000 ) ) ;
#8660 = CARTESIAN_POINT ( 'NONE',  ( 11.50231346626665996, 1.508968394323198847, 10.00000000000000000 ) ) ;
#8661 = FILL_AREA_STYLE_COLOUR ( '', #1995 ) ;
#8662 = CARTESIAN_POINT ( 'NONE',  ( -15.05755265055531034, -0.4891349978715467950, 3.747395293195558847E-16 ) ) ;
#8663 = CARTESIAN_POINT ( 'NONE',  ( 0.000000000000000000, 0.000000000000000000, 3.000000000000000000 ) ) ;
#8664 = COLOUR_RGB ( '', 0.09019608, 0.27058824, 0.51372549) ;
#8665 = ORIENTED_EDGE ( 'NONE', *, *, #10289, .T. ) ;
#8666 = CARTESIAN_POINT ( 'NONE',  ( 3.000000000000000888, 0.000000000000000000, 0.000000000000000000 ) ) ;
#8667 = ORIENTED_EDGE ( 'NONE', *, *, #11682, .F. ) ;
#8668 = DIRECTION ( 'NONE',  ( 0.000000000000000000, 0.4067366430758009299, -0.9135454576426005335 ) ) ;
#8669 = CARTESIAN_POINT ( 'NONE',  ( -0.1881845630465191765, -6.755137126427050553, 10.00000000000000000 ) ) ;
#8670 = AXIS2_PLACEMENT_3D ( 'NONE', #11390, #6551, #10285 ) ;
#8671 = LINE ( 'NONE', #271, #5252 ) ;
#8672 = CARTESIAN_POINT ( 'NONE',  ( 7.449730884303676248, -3.679036338562946096, 10.00000000000000000 ) ) ;
#8673 = CARTESIAN_POINT ( 'NONE',  ( 11.14370178440675474, -8.845034901279911210, 6.857782953271941950E-17 ) ) ;
#8674 =( LENGTH_UNIT ( ) NAMED_UNIT ( * ) SI_UNIT ( .MILLI., .METRE. ) );
#8675 = DIRECTION ( 'NONE',  ( -1.000000000000000000, -0.000000000000000000, 0.000000000000000000 ) ) ;
#8676 = ORIENTED_EDGE ( 'NONE', *, *, #9508, .T. ) ;
#8677 = AXIS2_PLACEMENT_3D ( 'NONE', #2932, #6593, #4769 ) ;
#8678 = EDGE_CURVE ( 'NONE', #2346, #2635, #1556, .T. ) ;
#8679 = ORIENTED_EDGE ( 'NONE', *, *, #4604, .T. ) ;
#8680 = DIRECTION ( 'NONE',  ( -1.000000000000000000, -0.000000000000000000, -0.000000000000000000 ) ) ;
#8681 = CARTESIAN_POINT ( 'NONE',  ( 3.000000000000000888, 9.667200211210106531, -20.86861857134724474 ) ) ;
#8682 = EDGE_CURVE ( 'NONE', #10975, #8500, #3708, .T. ) ;
#8683 = DIRECTION ( 'NONE',  ( 1.000000000000000000, 0.000000000000000000, 0.000000000000000000 ) ) ;
#8684 = DIRECTION ( 'NONE',  ( 0.000000000000000000, -1.000000000000000000, -1.048062100069321321E-14 ) ) ;
#8685 = CIRCLE ( 'NONE', #3410, 9.599999999999997868 ) ;
#8686 = AXIS2_PLACEMENT_3D ( 'NONE', #8849, #10735, #1437 ) ;
#8687 = CARTESIAN_POINT ( 'NONE',  ( -11.32214898804403802, 3.633524203738173419, 3.747395293195558847E-16 ) ) ;
#8688 = EDGE_CURVE ( 'NONE', #9879, #8749, #7751, .T. ) ;
#8689 = EDGE_CURVE ( 'NONE', #5268, #7198, #11430, .T. ) ;
#8690 = LINE ( 'NONE', #5691, #7629 ) ;
#8691 = ORIENTED_EDGE ( 'NONE', *, *, #6297, .F. ) ;
#8692 = ORIENTED_EDGE ( 'NONE', *, *, #9569, .F. ) ;
#8693 = EDGE_CURVE ( 'NONE', #5028, #1910, #5982, .T. ) ;
#8694 = SHAPE_DEFINITION_REPRESENTATION ( #10490, #8353 ) ;
#8695 = CARTESIAN_POINT ( 'NONE',  ( -6.864300873105356082, 13.92024697337932082, 10.00000000000000000 ) ) ;
#8696 = VERTEX_POINT ( 'NONE', #9893 ) ;
#8697 = AXIS2_PLACEMENT_3D ( 'NONE', #9740, #5090, #8835 ) ;
#8698 = CARTESIAN_POINT ( 'NONE',  ( 11.73504485001147124, -12.52947377801878837, 6.857782953271941950E-17 ) ) ;
#8699 = CARTESIAN_POINT ( 'NONE',  ( 1.500000000000000444, 1.556492618230968628, -24.75110766671650708 ) ) ;
#8700 = CARTESIAN_POINT ( 'NONE',  ( 3.000000000000000888, 13.28910708463127932, 20.93895013827586027 ) ) ;
#8701 = CARTESIAN_POINT ( 'NONE',  ( 0.000000000000000000, 0.000000000000000000, 1.000000000000000888 ) ) ;
#8702 = EDGE_LOOP ( 'NONE', ( #5977, #2192, #4368, #10150 ) ) ;
#8703 = CYLINDRICAL_SURFACE ( 'NONE', #844, 9.599999999999997868 ) ;
#8704 = CARTESIAN_POINT ( 'NONE',  ( 1.500000000000000444, -15.80756504416703656, 19.10918332567953115 ) ) ;
#8705 = CARTESIAN_POINT ( 'NONE',  ( -4.384918567263694555, -12.91535881965570631, 6.857782953271941950E-17 ) ) ;
#8706 = VERTEX_POINT ( 'NONE', #2425 ) ;
#8707 = DIRECTION ( 'NONE',  ( -1.000000000000000000, 0.000000000000000000, -0.000000000000000000 ) ) ;
#8708 = CARTESIAN_POINT ( 'NONE',  ( 0.000000000000000000, 20.86861857134747567, -9.667200211209610927 ) ) ;
#8709 = VERTEX_POINT ( 'NONE', #403 ) ;
#8710 = MANIFOLD_SOLID_BREP ( 'Extrude-Thin1', #1016 ) ;
#8711 = CARTESIAN_POINT ( 'NONE',  ( -1.307086582043127443, 11.26718560147321568, 10.00000000000000000 ) ) ;
#8712 = CARTESIAN_POINT ( 'NONE',  ( 3.000000000000000888, 22.42251312757886339, -5.117118920208268307 ) ) ;
#8713 = ORIENTED_EDGE ( 'NONE', *, *, #145, .F. ) ;
#8714 = DIRECTION ( 'NONE',  ( 0.000000000000000000, 0.000000000000000000, 1.000000000000000000 ) ) ;
#8715 = CARTESIAN_POINT ( 'NONE',  ( 3.000000000000000888, -4.135161237383403687, -24.45282072769605364 ) ) ;
#8716 = CARTESIAN_POINT ( 'NONE',  ( -12.27443204882852257, 3.949650873796767492, 10.00000000000000000 ) ) ;
#8717 = ADVANCED_FACE ( 'NONE', ( #9654 ), #10816, .T. ) ;
#8718 = LINE ( 'NONE', #11409, #2184 ) ;
#8719 = CARTESIAN_POINT ( 'NONE',  ( -15.00596061316373842, -1.728743269517114323, 3.747395293195558847E-16 ) ) ;
#8720 = FACE_OUTER_BOUND ( 'NONE', #5543, .T. ) ;
#8721 = CIRCLE ( 'NONE', #3829, 24.80000000000000071 ) ;
#8722 = CYLINDRICAL_SURFACE ( 'NONE', #9582, 9.599999999999997868 ) ;
#8723 = ORIENTED_EDGE ( 'NONE', *, *, #998, .F. ) ;
#8724 = EDGE_CURVE ( 'NONE', #3881, #11808, #10327, .T. ) ;
#8725 = ORIENTED_EDGE ( 'NONE', *, *, #6144, .F. ) ;
#8726 = FACE_OUTER_BOUND ( 'NONE', #3328, .T. ) ;
#8727 = CARTESIAN_POINT ( 'NONE',  ( 0.9209971296404340091, -6.773236541304583191, 10.00000000000000000 ) ) ;
#8728 = DIRECTION ( 'NONE',  ( 0.000000000000000000, 0.000000000000000000, -1.000000000000000000 ) ) ;
#8729 = CIRCLE ( 'NONE', #7335, 9.599999999999997868 ) ;
#8730 = CARTESIAN_POINT ( 'NONE',  ( 3.000000000000000888, 17.97274125076074114, 13.62355943574025652 ) ) ;
#8731 = CARTESIAN_POINT ( 'NONE',  ( -9.023584016175229650, 3.917288190900558131, 10.00000000000000000 ) ) ;
#8732 = CARTESIAN_POINT ( 'NONE',  ( -13.04979933117209256, -0.2127334381860506995, 6.857782953271941950E-17 ) ) ;
#8733 = PRESENTATION_STYLE_ASSIGNMENT (( #4016 ) ) ;
#8734 = DIRECTION ( 'NONE',  ( 0.000000000000000000, 0.000000000000000000, 1.000000000000000000 ) ) ;
#8735 = VERTEX_POINT ( 'NONE', #11609 ) ;
#8736 = CIRCLE ( 'NONE', #12041, 9.599999999999997868 ) ;
#8737 = EDGE_LOOP ( 'NONE', ( #5525, #3685, #10627, #5314 ) ) ;
#8738 = CYLINDRICAL_SURFACE ( 'NONE', #3576, 24.80000000000000071 ) ;
#8739 = DIRECTION ( 'NONE',  ( -1.000000000000000000, -0.000000000000000000, 0.000000000000000000 ) ) ;
#8740 = CARTESIAN_POINT ( 'NONE',  ( 0.000000000000000000, 19.75591328264886215, 10.87771529938168946 ) ) ;
#8741 = CARTESIAN_POINT ( 'NONE',  ( 0.000000000000000000, -19.10918332567968037, 15.80756504416684649 ) ) ;
#8742 = CARTESIAN_POINT ( 'NONE',  ( -4.622662292628548997, -8.344572748942098883, 3.747395293195558847E-16 ) ) ;
#8743 = SHAPE_REPRESENTATION ( 'BR-102', ( #5881, #3934, #3728, #1185, #2360, #5688, #7234 ), #3335 ) ;
#8744 = DIRECTION ( 'NONE',  ( 0.000000000000000000, -0.9945218953682721796, -0.1045284632676635878 ) ) ;
#8745 = VERTEX_POINT ( 'NONE', #1322 ) ;
#8746 = VERTEX_POINT ( 'NONE', #7124 ) ;
#8747 = PRODUCT_CONTEXT ( 'NONE', #3874, 'mechanical' ) ;
#8748 = CARTESIAN_POINT ( 'NONE',  ( 3.000000000000000888, 21.30300407174352983, 7.402892494506653875 ) ) ;
#8749 = VERTEX_POINT ( 'NONE', #7000 ) ;
#8750 = CARTESIAN_POINT ( 'NONE',  ( 3.000000000000000888, -17.71842311621541555, 17.35216073792435054 ) ) ;
#8751 = DIRECTION ( 'NONE',  ( 0.000000000000000000, 0.000000000000000000, 1.000000000000000000 ) ) ;
#8752 = DIRECTION ( 'NONE',  ( 0.000000000000000000, -0.8660254037844431485, 0.4999999999999920619 ) ) ;
#8753 = ORIENTED_EDGE ( 'NONE', *, *, #4582, .T. ) ;
#8754 = EDGE_CURVE ( 'NONE', #6571, #4657, #3103, .T. ) ;
#8755 = DIRECTION ( 'NONE',  ( -1.000000000000000000, 0.000000000000000000, -0.000000000000000000 ) ) ;
#8756 = EDGE_CURVE ( 'NONE', #2834, #4657, #1269, .T. ) ;
#8757 = EDGE_CURVE ( 'NONE', #277, #7198, #9930, .T. ) ;
#8758 = DIRECTION ( 'NONE',  ( -1.000000000000000000, 0.000000000000000000, 0.000000000000000000 ) ) ;
#8759 = CARTESIAN_POINT ( 'NONE',  ( -1.999398781552333526, 15.23274265415848916, 6.857782953271941950E-17 ) ) ;
#8760 = ORIENTED_EDGE ( 'NONE', *, *, #3169, .F. ) ;
#8761 = DIRECTION ( 'NONE',  ( -0.000000000000000000, -0.000000000000000000, 1.000000000000000000 ) ) ;
#8762 = VECTOR ( 'NONE', #2097, 1000.000000000000000 ) ;
#8763 = DIRECTION ( 'NONE',  ( 0.000000000000000000, 0.000000000000000000, 1.000000000000000000 ) ) ;
#8764 = ORIENTED_EDGE ( 'NONE', *, *, #5860, .F. ) ;
#8765 = CARTESIAN_POINT ( 'NONE',  ( -2.487495860704070250, -9.331140650584721641, 10.00000000000000000 ) ) ;
#8766 = ADVANCED_FACE ( 'NONE', ( #4149, #7063 ), #11549, .F. ) ;
#8767 = DIRECTION ( 'NONE',  ( 0.000000000000000000, 0.000000000000000000, 1.000000000000000000 ) ) ;
#8768 = FILL_AREA_STYLE_COLOUR ( '', #4515 ) ;
#8769 = VECTOR ( 'NONE', #10009, 1000.000000000000227 ) ;
#8770 = CARTESIAN_POINT ( 'NONE',  ( 0.000000000000000000, 0.000000000000000000, -15.00000000000000000 ) ) ;
#8771 =( GEOMETRIC_REPRESENTATION_CONTEXT ( 3 ) GLOBAL_UNCERTAINTY_ASSIGNED_CONTEXT ( ( #1336 ) ) GLOBAL_UNIT_ASSIGNED_CONTEXT ( ( #7812, #6036, #7985 ) ) REPRESENTATION_CONTEXT ( 'NONE', 'WORKASPACE' ) );
#8772 = DIRECTION ( 'NONE',  ( -1.000000000000000000, -0.000000000000000000, 0.000000000000000000 ) ) ;
#8773 = CARTESIAN_POINT ( 'NONE',  ( -9.546882484473293573, 8.373557015401750903, 10.00000000000000000 ) ) ;
#8774 = CARTESIAN_POINT ( 'NONE',  ( -4.793139000956299967, -14.90149022103882892, 3.747395293195558847E-16 ) ) ;
#8775 = DIRECTION ( 'NONE',  ( 0.000000000000000000, 0.3090169943749416781, 0.9510565162951555296 ) ) ;
#8776 = EDGE_CURVE ( 'NONE', #3303, #5937, #11885, .T. ) ;
#8777 = DIRECTION ( 'NONE',  ( -1.000000000000000000, -0.000000000000000000, 0.000000000000000000 ) ) ;
#8778 = VERTEX_POINT ( 'NONE', #3226 ) ;
#8779 = AXIS2_PLACEMENT_3D ( 'NONE', #3120, #11563, #2133 ) ;
#8780 = ORIENTED_EDGE ( 'NONE', *, *, #4086, .F. ) ;
#8781 = EDGE_CURVE ( 'NONE', #9635, #2061, #3884, .T. ) ;
#8782 = DIRECTION ( 'NONE',  ( -1.000000000000000000, -0.000000000000000000, -0.000000000000000000 ) ) ;
#8783 = DIRECTION ( 'NONE',  ( 1.000000000000000000, 0.000000000000000000, 0.000000000000000000 ) ) ;
#8784 = DIRECTION ( 'NONE',  ( -1.000000000000000000, 0.000000000000000000, 0.000000000000000000 ) ) ;
#8785 = CARTESIAN_POINT ( 'NONE',  ( -2.764021070441486039, -10.29567250283336399, 10.00000000000000000 ) ) ;
#8786 = AXIS2_PLACEMENT_3D ( 'NONE', #10208, #1144, #6711 ) ;
#8787 = CIRCLE ( 'NONE', #10930, 9.599999999999997868 ) ;
#8788 = CARTESIAN_POINT ( 'NONE',  ( 13.92981926110967450, -3.738495919395730116, 6.857782953271941950E-17 ) ) ;
#8789 = SURFACE_SIDE_STYLE ('',( #5917 ) ) ;
#8790 = EDGE_CURVE ( 'NONE', #6967, #8912, #6224, .T. ) ;
#8791 = DIRECTION ( 'NONE',  ( -1.000000000000000000, 0.000000000000000000, 0.000000000000000000 ) ) ;
#8792 = ORIENTED_EDGE ( 'NONE', *, *, #8247, .F. ) ;
#8793 = ORIENTED_EDGE ( 'NONE', *, *, #10247, .T. ) ;
#8794 = ORIENTED_EDGE ( 'NONE', *, *, #9908, .T. ) ;
#8795 = CARTESIAN_POINT ( 'NONE',  ( 0.000000000000000000, -7.432877647175055280, -21.76479567747249533 ) ) ;
#8796 = CARTESIAN_POINT ( 'NONE',  ( 16.25531780653859570, -2.690316503436296802, 10.00000000000000000 ) ) ;
#8797 = VECTOR ( 'NONE', #8923, 1000.000000000000000 ) ;
#8798 = CARTESIAN_POINT ( 'NONE',  ( 1.500000000000000444, 8.645255683529310176, -23.24434456306316577 ) ) ;
#8799 = EDGE_CURVE ( 'NONE', #3556, #4581, #2362, .T. ) ;
#8800 = CARTESIAN_POINT ( 'NONE',  ( -8.109405675832187299, 8.372220220304370741, 3.747395293195558847E-16 ) ) ;
#8801 = AXIS2_PLACEMENT_3D ( 'NONE', #2607, #10923, #9827 ) ;
#8802 = AXIS2_PLACEMENT_3D ( 'NONE', #198, #1305, #7733 ) ;
#8803 = CARTESIAN_POINT ( 'NONE',  ( 0.000000000000000000, 18.80635025205187816, -13.23915371906935867 ) ) ;
#8804 = ORIENTED_EDGE ( 'NONE', *, *, #3890, .T. ) ;
#8805 = ORIENTED_EDGE ( 'NONE', *, *, #9146, .T. ) ;
#8806 = CARTESIAN_POINT ( 'NONE',  ( 0.000000000000000000, 0.000000000000000000, 0.000000000000000000 ) ) ;
#8807 = CARTESIAN_POINT ( 'NONE',  ( -3.406233159845097891, 11.94786423299365197, 10.00000000000000000 ) ) ;
#8808 = VERTEX_POINT ( 'NONE', #1633 ) ;
#8809 = LINE ( 'NONE', #2198, #956 ) ;
#8810 = DIRECTION ( 'NONE',  ( 0.000000000000000000, 0.000000000000000000, 1.000000000000000000 ) ) ;
#8811 = AXIS2_PLACEMENT_3D ( 'NONE', #9744, #8840, #8896 ) ;
#8812 = UNCERTAINTY_MEASURE_WITH_UNIT (LENGTH_MEASURE( 1.000000000000000082E-05 ), #7845, 'distance_accuracy_value', 'NONE');
#8813 = CARTESIAN_POINT ( 'NONE',  ( 3.000000000000000888, 0.000000000000000000, 0.000000000000000000 ) ) ;
#8814 = AXIS2_PLACEMENT_3D ( 'NONE', #858, #1832, #5625 ) ;
#8815 = EDGE_LOOP ( 'NONE', ( #8553, #7972, #11634, #5870 ) ) ;
#8816 = AXIS2_PLACEMENT_3D ( 'NONE', #10169, #9319, #10236 ) ;
#8817 = CARTESIAN_POINT ( 'NONE',  ( 3.000000000000000888, 0.000000000000000000, 0.000000000000000000 ) ) ;
#8818 = FACE_OUTER_BOUND ( 'NONE', #4699, .T. ) ;
#8819 = CARTESIAN_POINT ( 'NONE',  ( -9.820986981721938847, 1.626514086989861108, 6.857782953271941950E-17 ) ) ;
#8820 = VERTEX_POINT ( 'NONE', #8240 ) ;
#8821 = CIRCLE ( 'NONE', #6850, 11.50000000000000178 ) ;
#8822 = CARTESIAN_POINT ( 'NONE',  ( 0.000000000000000000, 20.86861857134734421, 9.667200211209893368 ) ) ;
#8823 = VECTOR ( 'NONE', #6612, 1000.000000000000000 ) ;
#8824 = DIRECTION ( 'NONE',  ( 0.000000000000000000, 0.000000000000000000, -1.000000000000000000 ) ) ;
#8825 = VERTEX_POINT ( 'NONE', #8117 ) ;
#8826 = EDGE_CURVE ( 'NONE', #9539, #532, #2909, .T. ) ;
#8827 = CARTESIAN_POINT ( 'NONE',  ( -8.694522232909452697, -2.966707450564700643, 10.00000000000000000 ) ) ;
#8828 = ORIENTED_EDGE ( 'NONE', *, *, #10507, .T. ) ;
#8829 = CARTESIAN_POINT ( 'NONE',  ( 3.000000000000000888, 14.74749645580011226, 17.06259499759949705 ) ) ;
#8830 = ORIENTED_EDGE ( 'NONE', *, *, #904, .F. ) ;
#8831 = CIRCLE ( 'NONE', #4915, 22.99899999999999523 ) ;
#8832 = EDGE_CURVE ( 'NONE', #2073, #7721, #7182, .T. ) ;
#8833 = CARTESIAN_POINT ( 'NONE',  ( -22.00000000000000000, 0.000000000000000000, 20.00000000000000000 ) ) ;
#8834 =( GEOMETRIC_REPRESENTATION_CONTEXT ( 3 ) GLOBAL_UNCERTAINTY_ASSIGNED_CONTEXT ( ( #11855 ) ) GLOBAL_UNIT_ASSIGNED_CONTEXT ( ( #8674, #8450, #4073 ) ) REPRESENTATION_CONTEXT ( 'NONE', 'WORKASPACE' ) );
#8835 = DIRECTION ( 'NONE',  ( 0.000000000000000000, 0.000000000000000000, 1.000000000000000000 ) ) ;
#8836 = CARTESIAN_POINT ( 'NONE',  ( 8.143984375790578767, 3.063465613658708619, 10.00000000000000000 ) ) ;
#8837 = DIRECTION ( 'NONE',  ( 0.000000000000000000, 0.9510565162951521989, 0.3090169943749515036 ) ) ;
#8838 = DIRECTION ( 'NONE',  ( 0.000000000000000000, 0.000000000000000000, 1.000000000000000000 ) ) ;
#8839 = ADVANCED_FACE ( 'NONE', ( #894, #1812 ), #7244, .F. ) ;
#8840 = DIRECTION ( 'NONE',  ( -1.000000000000000000, -0.000000000000000000, -0.000000000000000000 ) ) ;
#8841 = VERTEX_POINT ( 'NONE', #6348 ) ;
#8842 = DIRECTION ( 'NONE',  ( 0.000000000000000000, 0.7431448254773954654, -0.6691306063588569053 ) ) ;
#8843 = EDGE_CURVE ( 'NONE', #11556, #916, #4630, .T. ) ;
#8844 =( GEOMETRIC_REPRESENTATION_CONTEXT ( 3 ) GLOBAL_UNCERTAINTY_ASSIGNED_CONTEXT ( ( #8932 ) ) GLOBAL_UNIT_ASSIGNED_CONTEXT ( ( #5960, #9687, #5037 ) ) REPRESENTATION_CONTEXT ( 'NONE', 'WORKASPACE' ) );
#8845 = ORIENTED_EDGE ( 'NONE', *, *, #7057, .T. ) ;
#8846 = AXIS2_PLACEMENT_3D ( 'NONE', #358, #4100, #7833 ) ;
#8847 = CARTESIAN_POINT ( 'NONE',  ( 3.000000000000000888, 14.74749645580034496, -17.06259499759930165 ) ) ;
#8848 = DIRECTION ( 'NONE',  ( 0.000000000000000000, 0.000000000000000000, 1.000000000000000000 ) ) ;
#8849 = CARTESIAN_POINT ( 'NONE',  ( 3.000000000000000888, 0.000000000000000000, 0.000000000000000000 ) ) ;
#8850 = CARTESIAN_POINT ( 'NONE',  ( 2.798030692817974341, 8.692477993603725750, 10.00000000000000000 ) ) ;
#8851 = STYLED_ITEM ( 'NONE', ( #4487 ), #323 ) ;
#8852 = CARTESIAN_POINT ( 'NONE',  ( 11.51680056346191883, -0.3781118375584790470, 6.857782953271941950E-17 ) ) ;
#8853 = DIRECTION ( 'NONE',  ( -1.000000000000000000, 0.000000000000000000, 0.000000000000000000 ) ) ;
#8854 = DIRECTION ( 'NONE',  ( 0.000000000000000000, 0.000000000000000000, -1.000000000000000000 ) ) ;
#8855 = ORIENTED_EDGE ( 'NONE', *, *, #4604, .F. ) ;
#8856 = ORIENTED_EDGE ( 'NONE', *, *, #2587, .F. ) ;
#8857 = VERTEX_POINT ( 'NONE', #5480 ) ;
#8858 = AXIS2_PLACEMENT_3D ( 'NONE', #4965, #6846, #7831 ) ;
#8859 = LINE ( 'NONE', #4081, #2180 ) ;
#8860 = CARTESIAN_POINT ( 'NONE',  ( 3.000000000000000888, 0.000000000000000000, 0.000000000000000000 ) ) ;
#8861 = CIRCLE ( 'NONE', #2206, 24.80000000000000071 ) ;
#8862 = FACE_OUTER_BOUND ( 'NONE', #4265, .T. ) ;
#8863 = CARTESIAN_POINT ( 'NONE',  ( 10.00611923916670953, -2.842981073525689517, 3.747395293195558847E-16 ) ) ;
#8864 = EDGE_CURVE ( 'NONE', #11729, #8857, #2123, .T. ) ;
#8865 = AXIS2_PLACEMENT_3D ( 'NONE', #2627, #2443, #7140 ) ;
#8866 = FACE_OUTER_BOUND ( 'NONE', #3688, .T. ) ;
#8867 = CARTESIAN_POINT ( 'NONE',  ( 3.000000000000000888, 10.87771529938162196, 19.75591328264889768 ) ) ;
#8868 = ORIENTED_EDGE ( 'NONE', *, *, #7934, .F. ) ;
#8869 = EDGE_LOOP ( 'NONE', ( #9425, #7455, #2906, #10339 ) ) ;
#8870 = VECTOR ( 'NONE', #1225, 1000.000000000000000 ) ;
#8871 = CARTESIAN_POINT ( 'NONE',  ( -1.124919223378054722, -13.71093750358708796, 10.00000000000000000 ) ) ;
#8872 = ORIENTED_EDGE ( 'NONE', *, *, #8008, .T. ) ;
#8873 = DIRECTION ( 'NONE',  ( 0.000000000000000000, 0.000000000000000000, 1.000000000000000000 ) ) ;
#8874 = DIRECTION ( 'NONE',  ( -1.000000000000000000, -0.000000000000000000, 0.000000000000000000 ) ) ;
#8875 = ADVANCED_FACE ( 'NONE', ( #9216 ), #8361, .T. ) ;
#8876 = CIRCLE ( 'NONE', #8296, 19.00000000000000000 ) ;
#8877 = DIRECTION ( 'NONE',  ( -1.000000000000000000, 0.000000000000000000, 0.000000000000000000 ) ) ;
#8878 = ORIENTED_EDGE ( 'NONE', *, *, #7814, .F. ) ;
#8879 = FACE_BOUND ( 'NONE', #659, .T. ) ;
#8880 = LINE ( 'NONE', #484, #11957 ) ;
#8881 = CARTESIAN_POINT ( 'NONE',  ( 8.329772390959197637, 2.373743296044066309, 6.857782953271941950E-17 ) ) ;
#8882 = EDGE_LOOP ( 'NONE', ( #164, #10614, #2405, #3167 ) ) ;
#8883 = DIRECTION ( 'NONE',  ( -1.000000000000000000, 0.000000000000000000, 0.000000000000000000 ) ) ;
#8884 = AXIS2_PLACEMENT_3D ( 'NONE', #10423, #5837, #10357 ) ;
#8885 = DIRECTION ( 'NONE',  ( -1.000000000000000000, 0.000000000000000000, 0.000000000000000000 ) ) ;
#8886 = VERTEX_POINT ( 'NONE', #10070 ) ;
#8887 = CARTESIAN_POINT ( 'NONE',  ( -6.777230418910823673, -10.52530689671158548, 10.00000000000000000 ) ) ;
#8888 = CARTESIAN_POINT ( 'NONE',  ( 0.000000000000000000, -11.79560690673886292, 19.74380051311536022 ) ) ;
#8889 = EDGE_LOOP ( 'NONE', ( #1686, #5634, #1547, #8934 ) ) ;
#8890 = AXIS2_PLACEMENT_3D ( 'NONE', #1421, #8772, #5153 ) ;
#8891 = CARTESIAN_POINT ( 'NONE',  ( 0.000000000000000000, 0.000000000000000000, 3.000000000000000000 ) ) ;
#8892 = CYLINDRICAL_SURFACE ( 'NONE', #7906, 22.99899999999999878 ) ;
#8893 = CARTESIAN_POINT ( 'NONE',  ( 8.527474615971327054, 0.9793716136081388468, 10.00000000000000000 ) ) ;
#8894 = CARTESIAN_POINT ( 'NONE',  ( 1.500000000000000444, 19.43515443678423793, -15.40502424595126030 ) ) ;
#8895 = CARTESIAN_POINT ( 'NONE',  ( -11.15100792855598755, -5.055838994807843711, 3.747395293195558847E-16 ) ) ;
#8896 = DIRECTION ( 'NONE',  ( 0.000000000000000000, 0.000000000000000000, 1.000000000000000000 ) ) ;
#8897 = VERTEX_POINT ( 'NONE', #1567 ) ;
#8898 = CARTESIAN_POINT ( 'NONE',  ( 3.000000000000000888, -1.901833551798098876, -22.47229024614979309 ) ) ;
#8899 = EDGE_LOOP ( 'NONE', ( #6454, #3413, #3481, #6974 ) ) ;
#8900 = ADVANCED_FACE ( 'NONE', ( #5304 ), #1690, .T. ) ;
#8901 = LINE ( 'NONE', #2345, #2650 ) ;
#8902 = VERTEX_POINT ( 'NONE', #9040 ) ;
#8903 = DIRECTION ( 'NONE',  ( 0.000000000000000000, 0.8090169943749446757, 0.5877852522924770229 ) ) ;
#8904 = EDGE_CURVE ( 'NONE', #1329, #9017, #3291, .T. ) ;
#8905 = FACE_OUTER_BOUND ( 'NONE', #7548, .T. ) ;
#8906 = CARTESIAN_POINT ( 'NONE',  ( 0.000000000000000000, 0.000000000000000000, 1.000000000000000888 ) ) ;
#8907 = CARTESIAN_POINT ( 'NONE',  ( 5.247589697392150754, -6.187652788349034871, 10.00000000000000000 ) ) ;
#8908 = CARTESIAN_POINT ( 'NONE',  ( -5.965338750500049692, 7.524205049158500636, 6.857782953271941950E-17 ) ) ;
#8909 = CYLINDRICAL_SURFACE ( 'NONE', #11176, 24.80000000000000071 ) ;
#8910 = ADVANCED_FACE ( 'NONE', ( #10931 ), #766, .T. ) ;
#8911 = DIRECTION ( 'NONE',  ( 1.000000000000000000, 0.000000000000000000, 0.000000000000000000 ) ) ;
#8912 = VERTEX_POINT ( 'NONE', #7366 ) ;
#8913 = ORIENTED_EDGE ( 'NONE', *, *, #8179, .T. ) ;
#8914 = VERTEX_POINT ( 'NONE', #1743 ) ;
#8915 = AXIS2_PLACEMENT_3D ( 'NONE', #11460, #1064, #4794 ) ;
#8916 = CARTESIAN_POINT ( 'NONE',  ( -4.793139000956300855, -14.90149022103883247, 10.00000000000000000 ) ) ;
#8917 = EDGE_CURVE ( 'NONE', #2390, #1768, #9351, .T. ) ;
#8918 = DIRECTION ( 'NONE',  ( 0.000000000000000000, 0.000000000000000000, -1.000000000000000000 ) ) ;
#8919 = CARTESIAN_POINT ( 'NONE',  ( 3.000000000000000888, 13.62355943574019435, 17.97274125076078732 ) ) ;
#8920 = CARTESIAN_POINT ( 'NONE',  ( 0.9209971296404340091, -6.773236541304579639, 3.747395293195558847E-16 ) ) ;
#8921 = CARTESIAN_POINT ( 'NONE',  ( 0.000000000000000000, 16.85990652506900389, 15.64281154287603215 ) ) ;
#8922 = VECTOR ( 'NONE', #9722, 1000.000000000000000 ) ;
#8923 = DIRECTION ( 'NONE',  ( -1.000000000000000000, 0.000000000000000000, -0.000000000000000000 ) ) ;
#8924 = ORIENTED_EDGE ( 'NONE', *, *, #4834, .F. ) ;
#8925 = ORIENTED_EDGE ( 'NONE', *, *, #5461, .T. ) ;
#8926 = CARTESIAN_POINT ( 'NONE',  ( 11.14370178440676007, -8.845034901279914763, 10.00000000000000000 ) ) ;
#8927 = VERTEX_POINT ( 'NONE', #835 ) ;
#8928 = DIRECTION ( 'NONE',  ( 0.000000000000000000, -0.9781476007338079093, 0.2079116908177492118 ) ) ;
#8929 = DIRECTION ( 'NONE',  ( -1.000000000000000000, 0.000000000000000000, -0.000000000000000000 ) ) ;
#8930 = DIRECTION ( 'NONE',  ( -1.000000000000000000, -0.000000000000000000, 0.000000000000000000 ) ) ;
#8931 = EDGE_CURVE ( 'NONE', #9548, #7191, #2710, .T. ) ;
#8932 = UNCERTAINTY_MEASURE_WITH_UNIT (LENGTH_MEASURE( 1.000000000000000082E-05 ), #5960, 'distance_accuracy_value', 'NONE');
#8933 = CARTESIAN_POINT ( 'NONE',  ( 3.000000000000000888, 22.99643626497956816, 0.3433949777332492848 ) ) ;
#8934 = ORIENTED_EDGE ( 'NONE', *, *, #11197, .T. ) ;
#8935 = PLANE ( 'NONE',  #11606 ) ;
#8936 = CARTESIAN_POINT ( 'NONE',  ( 3.000000000000000888, 22.56530478845649057, 4.445336973060936891 ) ) ;
#8937 = CARTESIAN_POINT ( 'NONE',  ( -9.386162357322611172, -4.067606288967436257, 6.857782953271941950E-17 ) ) ;
#8938 = EDGE_CURVE ( 'NONE', #3562, #10640, #9097, .T. ) ;
#8939 = CARTESIAN_POINT ( 'NONE',  ( 3.000000000000000888, -12.88318129270191825, 18.51065745848373822 ) ) ;
#8940 = CARTESIAN_POINT ( 'NONE',  ( 3.000000000000000888, 17.31945870441167301, -15.13242714128102406 ) ) ;
#8941 = ORIENTED_EDGE ( 'NONE', *, *, #4492, .F. ) ;
#8942 = CARTESIAN_POINT ( 'NONE',  ( -11.74902089294173813, -3.156991809147611683, 10.00000000000000000 ) ) ;
#8943 = ORIENTED_EDGE ( 'NONE', *, *, #7185, .F. ) ;
#8944 = CARTESIAN_POINT ( 'NONE',  ( 3.000000000000000888, 20.08719549084880640, -11.20082935824054182 ) ) ;
#8945 = CYLINDRICAL_SURFACE ( 'NONE', #6603, 9.599999999999997868 ) ;
#8946 = DIRECTION ( 'NONE',  ( -1.000000000000000000, 0.000000000000000000, -0.000000000000000000 ) ) ;
#8947 = CARTESIAN_POINT ( 'NONE',  ( 1.661435237661583297, -7.700870200009183542, 10.00000000000000000 ) ) ;
#8948 = EDGE_CURVE ( 'NONE', #7092, #1140, #11110, .T. ) ;
#8949 = CIRCLE ( 'NONE', #3274, 9.599999999999996092 ) ;
#8950 = CARTESIAN_POINT ( 'NONE',  ( 3.000000000000000888, -15.42759117534397006, 16.45023496161660148 ) ) ;
#8951 = CARTESIAN_POINT ( 'NONE',  ( -10.51222845931327576, 5.388985543800765221, 3.747395293195558847E-16 ) ) ;
#8952 = CARTESIAN_POINT ( 'NONE',  ( 3.000000000000000888, 22.37663021667340146, 2.811977935938166695 ) ) ;
#8953 = ORIENTED_EDGE ( 'NONE', *, *, #5019, .T. ) ;
#8954 = CARTESIAN_POINT ( 'NONE',  ( 0.000000000000000000, 0.000000000000000000, 0.000000000000000000 ) ) ;
#8955 = ORIENTED_EDGE ( 'NONE', *, *, #9947, .F. ) ;
#8956 = CARTESIAN_POINT ( 'NONE',  ( -10.00000000000000000, 0.000000000000000000, 0.000000000000000000 ) ) ;
#8957 = ORIENTED_EDGE ( 'NONE', *, *, #9496, .T. ) ;
#8958 = CARTESIAN_POINT ( 'NONE',  ( 3.000000000000000888, -22.54798042742718422, 0.4575788569251160731 ) ) ;
#8959 = DIRECTION ( 'NONE',  ( -1.000000000000000000, 0.000000000000000000, 0.000000000000000000 ) ) ;
#8960 = FACE_OUTER_BOUND ( 'NONE', #5588, .T. ) ;
#8961 = LINE ( 'NONE', #572, #7047 ) ;
#8962 = CARTESIAN_POINT ( 'NONE',  ( 2.084091085258986009, 8.931495281877380066, 6.857782953271941950E-17 ) ) ;
#8963 = DIRECTION ( 'NONE',  ( 0.000000000000000000, 0.000000000000000000, 1.000000000000000000 ) ) ;
#8964 = VECTOR ( 'NONE', #836, 1000.000000000000000 ) ;
#8965 = DIRECTION ( 'NONE',  ( 0.000000000000000000, 0.8090169943749485615, -0.5877852522924714718 ) ) ;
#8966 = VERTEX_POINT ( 'NONE', #10125 ) ;
#8967 = CIRCLE ( 'NONE', #10911, 24.80000000000000071 ) ;
#8968 = ORIENTED_EDGE ( 'NONE', *, *, #3754, .T. ) ;
#8969 = EDGE_CURVE ( 'NONE', #4541, #7118, #6611, .T. ) ;
#8970 = VERTEX_POINT ( 'NONE', #3649 ) ;
#8971 = CARTESIAN_POINT ( 'NONE',  ( 9.623054350189521600, -9.012277985855607909, 10.00000000000000000 ) ) ;
#8972 = EDGE_CURVE ( 'NONE', #4987, #3516, #8377, .T. ) ;
#8973 = CIRCLE ( 'NONE', #7801, 22.99899999999999878 ) ;
#8974 = CARTESIAN_POINT ( 'NONE',  ( 3.000000000000000000, 0.000000000000000000, 0.000000000000000000 ) ) ;
#8975 = CARTESIAN_POINT ( 'NONE',  ( -8.962830026514755133, 0.7152994853347065529, 3.747395293195558847E-16 ) ) ;
#8976 = DIRECTION ( 'NONE',  ( 0.000000000000000000, 0.000000000000000000, 1.000000000000000000 ) ) ;
#8978 = ADVANCED_FACE ( 'NONE', ( #5666 ), #3954, .T. ) ;
#8977 = CIRCLE ( 'NONE', #10737, 22.99900000000000233 ) ;
#8979 = CARTESIAN_POINT ( 'NONE',  ( 0.000000000000000000, -23.05871956130128808, 9.128825345752948905 ) ) ;
#8980 = VECTOR ( 'NONE', #11370, 1000.000000000000000 ) ;
#8981 = ORIENTED_EDGE ( 'NONE', *, *, #587, .T. ) ;
#8982 = CARTESIAN_POINT ( 'NONE',  ( 2.259453438922059298, -13.68937604509904737, 10.00000000000000000 ) ) ;
#8983 = EDGE_CURVE ( 'NONE', #6466, #7118, #8967, .T. ) ;
#8984 = VECTOR ( 'NONE', #2555, 1000.000000000000000 ) ;
#8985 = ORIENTED_EDGE ( 'NONE', *, *, #3326, .T. ) ;
#8986 = CARTESIAN_POINT ( 'NONE',  ( 1.445324715877977173, -3.701599742324200637, 10.00000000000000000 ) ) ;
#8987 = CARTESIAN_POINT ( 'NONE',  ( 0.000000000000000000, -21.97817939804047427, 11.48910920600676100 ) ) ;
#8988 = CARTESIAN_POINT ( 'NONE',  ( 1.500000000000000444, -13.72351598154883412, -20.65684170206505499 ) ) ;
#8989 = DIRECTION ( 'NONE',  ( 0.000000000000000000, 0.000000000000000000, 1.000000000000000000 ) ) ;
#8990 = ORIENTED_EDGE ( 'NONE', *, *, #3594, .F. ) ;
#8991 = DIRECTION ( 'NONE',  ( -1.000000000000000000, 0.000000000000000000, 0.000000000000000000 ) ) ;
#8992 = AXIS2_PLACEMENT_3D ( 'NONE', #5405, #563, #9989 ) ;
#8993 = DIRECTION ( 'NONE',  ( -1.000000000000000000, 0.000000000000000000, 0.000000000000000000 ) ) ;
#8994 = CARTESIAN_POINT ( 'NONE',  ( 5.343773788080180331, 10.82393792025543711, 6.857782953271941950E-17 ) ) ;
#8995 = DIRECTION ( 'NONE',  ( -1.000000000000000000, 0.000000000000000000, -0.000000000000000000 ) ) ;
#8996 = ORIENTED_EDGE ( 'NONE', *, *, #4943, .T. ) ;
#8997 = CARTESIAN_POINT ( 'NONE',  ( 3.000000000000000888, -4.445336973060693531, -22.56530478845653676 ) ) ;
#8998 = CIRCLE ( 'NONE', #1179, 22.00000000000000000 ) ;
#8999 = ORIENTED_EDGE ( 'NONE', *, *, #3214, .T. ) ;
#9000 = AXIS2_PLACEMENT_3D ( 'NONE', #5261, #9858, #9969 ) ;
#9001 = CARTESIAN_POINT ( 'NONE',  ( 2.581500635392915299, -6.456130005640037695, 10.00000000000000000 ) ) ;
#9002 = CIRCLE ( 'NONE', #2745, 9.599999999999999645 ) ;
#9003 = ORIENTED_EDGE ( 'NONE', *, *, #1873, .F. ) ;
#9004 = CARTESIAN_POINT ( 'NONE',  ( 3.000000000000000888, -1.039229259764315128, -24.77821629063822684 ) ) ;
#9005 = PRESENTATION_LAYER_ASSIGNMENT (  '', '', ( #9786 ) ) ;
#9006 = ORIENTED_EDGE ( 'NONE', *, *, #10108, .T. ) ;
#9007 = CARTESIAN_POINT ( 'NONE',  ( 3.000000000000000888, 0.000000000000000000, 0.000000000000000000 ) ) ;
#9008 = CARTESIAN_POINT ( 'NONE',  ( 3.000000000000000888, -21.14796121233190362, -9.039786367039052806 ) ) ;
#9009 = CARTESIAN_POINT ( 'NONE',  ( -0.1814876354083667931, -10.77628937513455654, 10.00000000000000000 ) ) ;
#9010 = CIRCLE ( 'NONE', #3545, 9.599999999999996092 ) ;
#9011 = DIRECTION ( 'NONE',  ( -1.000000000000000000, 0.000000000000000000, -0.000000000000000000 ) ) ;
#9012 = CARTESIAN_POINT ( 'NONE',  ( 1.050035089571674352, -12.78847817906846096, 3.747395293195558847E-16 ) ) ;
#9013 = CIRCLE ( 'NONE', #8439, 22.99899999999999523 ) ;
#9014 = ADVANCED_FACE ( 'NONE', ( #5605 ), #2856, .T. ) ;
#9015 = DIRECTION ( 'NONE',  ( -1.000000000000000000, 0.000000000000000000, -0.000000000000000000 ) ) ;
#9016 = ORIENTED_EDGE ( 'NONE', *, *, #8380, .F. ) ;
#9017 = VERTEX_POINT ( 'NONE', #4690 ) ;
#9018 = CARTESIAN_POINT ( 'NONE',  ( 3.000000000000000888, -17.06259499759954679, 14.74749645580005364 ) ) ;
#9019 = VERTEX_POINT ( 'NONE', #7610 ) ;
#9020 = CARTESIAN_POINT ( 'NONE',  ( 0.000000000000000000, 0.000000000000000000, -15.00000000000000000 ) ) ;
#9021 = AXIS2_PLACEMENT_3D ( 'NONE', #7171, #11889, #5466 ) ;
#9022 = CIRCLE ( 'NONE', #4502, 19.99999999999999645 ) ;
#9023 = DIRECTION ( 'NONE',  ( 0.000000000000000000, -0.9510565162951503115, -0.3090169943749572767 ) ) ;
#9024 = ORIENTED_EDGE ( 'NONE', *, *, #5338, .F. ) ;
#9025 = EDGE_CURVE ( 'NONE', #7701, #5043, #4932, .T. ) ;
#9026 = AXIS2_PLACEMENT_3D ( 'NONE', #7516, #4938, #3099 ) ;
#9027 = FACE_OUTER_BOUND ( 'NONE', #519, .T. ) ;
#9028 = DIRECTION ( 'NONE',  ( 0.000000000000000000, 0.000000000000000000, -1.000000000000000000 ) ) ;
#9029 = CARTESIAN_POINT ( 'NONE',  ( 0.000000000000000000, 0.000000000000000000, 0.000000000000000000 ) ) ;
#9030 = CARTESIAN_POINT ( 'NONE',  ( -6.589974825828272209, 7.038139701356662670, 6.857782953271941950E-17 ) ) ;
#9031 = DIRECTION ( 'NONE',  ( 1.000000000000000000, 0.000000000000000000, 0.000000000000000000 ) ) ;
#9032 = CARTESIAN_POINT ( 'NONE',  ( 1.499999999999999556, -22.21333432029571142, 11.02759168516737276 ) ) ;
#9033 = ORIENTED_EDGE ( 'NONE', *, *, #10061, .T. ) ;
#9034 = CIRCLE ( 'NONE', #8425, 9.599999999999997868 ) ;
#9035 = VERTEX_POINT ( 'NONE', #3041 ) ;
#9036 = ORIENTED_EDGE ( 'NONE', *, *, #904, .T. ) ;
#9037 = CARTESIAN_POINT ( 'NONE',  ( -11.92955594661033558, -2.174140050202246766, 10.00000000000000000 ) ) ;
#9038 = VECTOR ( 'NONE', #11087, 1000.000000000000000 ) ;
#9039 = CIRCLE ( 'NONE', #41, 22.99899999999999878 ) ;
#9040 = CARTESIAN_POINT ( 'NONE',  ( 0.000000000000000000, -15.64281154287608722, 16.85990652506894705 ) ) ;
#9041 = DIRECTION ( 'NONE',  ( -1.000000000000000000, -0.000000000000000000, -0.000000000000000000 ) ) ;
#9042 = CARTESIAN_POINT ( 'NONE',  ( -5.069009347565034851, 2.772702716244574095, 3.747395293195558847E-16 ) ) ;
#9043 = DIRECTION ( 'NONE',  ( 0.000000000000000000, 0.000000000000000000, 1.000000000000000000 ) ) ;
#9044 = CARTESIAN_POINT ( 'NONE',  ( 0.000000000000000000, -24.75110766671653195, 1.556492618230558289 ) ) ;
#9045 = EDGE_LOOP ( 'NONE', ( #3928, #3674, #2835, #597 ) ) ;
#9046 = ORIENTED_EDGE ( 'NONE', *, *, #11809, .T. ) ;
#9047 = EDGE_LOOP ( 'NONE', ( #6383, #10251, #4044, #10956 ) ) ;
#9048 = CARTESIAN_POINT ( 'NONE',  ( -10.00000000000000000, 0.000000000000000000, 0.000000000000000000 ) ) ;
#9049 = ADVANCED_FACE ( 'NONE', ( #89 ), #9517, .T. ) ;
#9050 = CIRCLE ( 'NONE', #3780, 24.80000000000000071 ) ;
#9051 = CARTESIAN_POINT ( 'NONE',  ( 3.000000000000000888, -21.97817939804047427, 11.48910920600676100 ) ) ;
#9052 = CARTESIAN_POINT ( 'NONE',  ( 1.500000000000000444, -17.71842311621518462, -17.35216073792458857 ) ) ;
#9053 = ORIENTED_EDGE ( 'NONE', *, *, #11773, .F. ) ;
#9054 = PRODUCT_DEFINITION ( 'UNKNOWN', '', #3922, #1584 ) ;
#9055 = CIRCLE ( 'NONE', #6120, 22.99899999999999878 ) ;
#9056 = LINE ( 'NONE', #8004, #3589 ) ;
#9057 = EDGE_CURVE ( 'NONE', #215, #4173, #4462, .T. ) ;
#9058 = CARTESIAN_POINT ( 'NONE',  ( 3.000000000000000888, 0.000000000000000000, 0.000000000000000000 ) ) ;
#9059 = CARTESIAN_POINT ( 'NONE',  ( 1.597090680284417363, 12.12373805211590749, 6.857782953271941950E-17 ) ) ;
#9060 = AXIS2_PLACEMENT_3D ( 'NONE', #1086, #3899, #9229 ) ;
#9061 = CIRCLE ( 'NONE', #6516, 22.99899999999999878 ) ;
#9062 = ADVANCED_FACE ( 'NONE', ( #10257 ), #6523, .T. ) ;
#9063 = CARTESIAN_POINT ( 'NONE',  ( 3.000000000000000888, 21.96011696265484403, 5.135568396240393518 ) ) ;
#9064 = VERTEX_POINT ( 'NONE', #7681 ) ;
#9065 = CARTESIAN_POINT ( 'NONE',  ( 3.000000000000000888, 0.000000000000000000, 0.000000000000000000 ) ) ;
#9066 = ORIENTED_EDGE ( 'NONE', *, *, #8157, .F. ) ;
#9067 = AXIS2_PLACEMENT_3D ( 'NONE', #4458, #11067, #9476 ) ;
#9068 = ORIENTED_EDGE ( 'NONE', *, *, #6404, .T. ) ;
#9069 = CARTESIAN_POINT ( 'NONE',  ( -5.846204292276370396, 1.022993486932170404, 10.00000000000000000 ) ) ;
#9070 = CARTESIAN_POINT ( 'NONE',  ( 0.000000000000000000, 17.06259499759944021, 14.74749645580017088 ) ) ;
#9071 = VERTEX_POINT ( 'NONE', #205 ) ;
#9072 = CARTESIAN_POINT ( 'NONE',  ( 3.000000000000002665, 0.000000000000000000, 0.000000000000000000 ) ) ;
#9073 = DIRECTION ( 'NONE',  ( -1.000000000000000000, 0.000000000000000000, 0.000000000000000000 ) ) ;
#9074 = CARTESIAN_POINT ( 'NONE',  ( 4.698850784960275639, -6.565226861933597391, 10.00000000000000000 ) ) ;
#9075 = VECTOR ( 'NONE', #7628, 1000.000000000000000 ) ;
#9076 = CYLINDRICAL_SURFACE ( 'NONE', #1216, 9.599999999999997868 ) ;
#9077 = LINE ( 'NONE', #7158, #790 ) ;
#9078 = VERTEX_POINT ( 'NONE', #1870 ) ;
#9079 = EDGE_LOOP ( 'NONE', ( #2515, #3150, #10005, #9158 ) ) ;
#9080 = CYLINDRICAL_SURFACE ( 'NONE', #5479, 22.99899999999999878 ) ;
#9081 = VERTEX_POINT ( 'NONE', #2913 ) ;
#9082 = EDGE_CURVE ( 'NONE', #3896, #4836, #5851, .T. ) ;
#9083 = CARTESIAN_POINT ( 'NONE',  ( -4.428608208598374674, -4.627450663480007442, 3.747395293195558847E-16 ) ) ;
#9084 = LINE ( 'NONE', #2652, #4402 ) ;
#9085 = ORIENTED_EDGE ( 'NONE', *, *, #5642, .F. ) ;
#9086 = EDGE_CURVE ( 'NONE', #9844, #2082, #10437, .T. ) ;
#9087 = CARTESIAN_POINT ( 'NONE',  ( -10.00000000000000000, 0.000000000000000000, 0.000000000000000000 ) ) ;
#9088 = CARTESIAN_POINT ( 'NONE',  ( 3.000000000000000888, -8.645255683528844770, -23.24434456306333985 ) ) ;
#9089 = CARTESIAN_POINT ( 'NONE',  ( 1.018538006779725835, -7.771884277300785904, 10.00000000000000000 ) ) ;
#9090 = CARTESIAN_POINT ( 'NONE',  ( -6.506554845699739076, -8.196137552275128968, 6.857782953271941950E-17 ) ) ;
#9091 = DIRECTION ( 'NONE',  ( 0.000000000000000000, 0.000000000000000000, 1.000000000000000000 ) ) ;
#9092 = CYLINDRICAL_SURFACE ( 'NONE', #416, 22.99899999999999878 ) ;
#9093 = EDGE_LOOP ( 'NONE', ( #9274, #4010, #12076, #7659 ) ) ;
#9094 = EDGE_CURVE ( 'NONE', #6369, #4549, #9361, .T. ) ;
#9095 = ORIENTED_EDGE ( 'NONE', *, *, #7632, .T. ) ;
#9096 = CARTESIAN_POINT ( 'NONE',  ( 7.081399987883182590, -10.98142027556026967, 10.00000000000000000 ) ) ;
#9097 = LINE ( 'NONE', #5422, #4863 ) ;
#9098 = DIRECTION ( 'NONE',  ( 0.000000000000000000, 0.000000000000000000, 1.000000000000000000 ) ) ;
#9099 = AXIS2_PLACEMENT_3D ( 'NONE', #7227, #693, #635 ) ;
#9100 = CARTESIAN_POINT ( 'NONE',  ( -5.315861670734002509, 2.363279591655833567, 3.747395293195558847E-16 ) ) ;
#9101 = DIRECTION ( 'NONE',  ( 1.000000000000000000, 0.000000000000000000, 0.000000000000000000 ) ) ;
#9102 = LINE ( 'NONE', #6631, #389 ) ;
#9103 = ORIENTED_EDGE ( 'NONE', *, *, #6805, .F. ) ;
#9104 = ORIENTED_EDGE ( 'NONE', *, *, #10715, .F. ) ;
#9105 = AXIS2_PLACEMENT_3D ( 'NONE', #3080, #6798, #5030 ) ;
#9106 = SHAPE_DEFINITION_REPRESENTATION ( #11470, #5127 ) ;
#9107 = ORIENTED_EDGE ( 'NONE', *, *, #4255, .F. ) ;
#9108 = CARTESIAN_POINT ( 'NONE',  ( 3.194803811556594653, -2.743189786380181072, 10.00000000000000000 ) ) ;
#9109 = DIRECTION ( 'NONE',  ( 0.000000000000000000, 0.000000000000000000, -1.000000000000000000 ) ) ;
#9110 = CYLINDRICAL_SURFACE ( 'NONE', #3259, 3.500000000000000000 ) ;
#9111 = DIRECTION ( 'NONE',  ( 0.000000000000000000, 0.1045284632676470038, 0.9945218953682740670 ) ) ;
#9112 = AXIS2_PLACEMENT_3D ( 'NONE', #9485, #7580, #8516 ) ;
#9113 = DIRECTION ( 'NONE',  ( -1.000000000000000000, 0.000000000000000000, -0.000000000000000000 ) ) ;
#9114 = CARTESIAN_POINT ( 'NONE',  ( -7.014275365397503847, 0.1192422097806469378, 6.857782953271941950E-17 ) ) ;
#9115 = DIRECTION ( 'NONE',  ( 1.000000000000000000, -0.000000000000000000, 0.000000000000000000 ) ) ;
#9116 = CARTESIAN_POINT ( 'NONE',  ( 3.000000000000000888, 0.000000000000000000, 0.000000000000000000 ) ) ;
#9117 = ORIENTED_EDGE ( 'NONE', *, *, #11747, .T. ) ;
#9118 = VERTEX_POINT ( 'NONE', #10373 ) ;
#9119 = VECTOR ( 'NONE', #5322, 1000.000000000000000 ) ;
#9120 = CARTESIAN_POINT ( 'NONE',  ( -8.409270314015810044, 2.833341551407463133, 10.00000000000000000 ) ) ;
#9121 = EDGE_CURVE ( 'NONE', #7873, #6662, #8671, .T. ) ;
#9122 = ORIENTED_EDGE ( 'NONE', *, *, #4570, .F. ) ;
#9123 = DIRECTION ( 'NONE',  ( 0.000000000000000000, -0.9781476007338034684, -0.2079116908177699174 ) ) ;
#9124 = ORIENTED_EDGE ( 'NONE', *, *, #1670, .F. ) ;
#9125 = EDGE_CURVE ( 'NONE', #8629, #2147, #957, .T. ) ;
#9126 = DIRECTION ( 'NONE',  ( 0.000000000000000000, -0.5877852522924797984, 0.8090169943749425663 ) ) ;
#9127 = DIRECTION ( 'NONE',  ( -1.000000000000000000, 0.000000000000000000, 0.000000000000000000 ) ) ;
#9128 = CARTESIAN_POINT ( 'NONE',  ( -7.040021908109685533, -0.4595208068205508534, 10.00000000000000000 ) ) ;
#9129 = CARTESIAN_POINT ( 'NONE',  ( 3.000000000000000888, -22.15038895030651744, 4.240409074144028345 ) ) ;
#9130 = CYLINDRICAL_SURFACE ( 'NONE', #11935, 22.99899999999999878 ) ;
#9131 = EDGE_LOOP ( 'NONE', ( #732, #9753, #12061, #7872 ) ) ;
#9132 = CARTESIAN_POINT ( 'NONE',  ( 0.000000000000000000, -19.29833442572367375, 11.67026512804540950 ) ) ;
#9133 = ORIENTED_EDGE ( 'NONE', *, *, #2305, .T. ) ;
#9134 = EDGE_CURVE ( 'NONE', #117, #1630, #7194, .T. ) ;
#9135 = CARTESIAN_POINT ( 'NONE',  ( 5.211919109253432936, 5.981019939437269173, 3.747395293195558847E-16 ) ) ;
#9136 = CARTESIAN_POINT ( 'NONE',  ( -10.00000000000000000, 0.000000000000000000, 0.000000000000000000 ) ) ;
#9137 = VERTEX_POINT ( 'NONE', #8428 ) ;
#9138 = CARTESIAN_POINT ( 'NONE',  ( 0.000000000000000000, 22.56530478845654386, -4.445336973060635799 ) ) ;
#9139 = CARTESIAN_POINT ( 'NONE',  ( 1.500000000000000444, 22.21333432029563681, 11.02759168516753085 ) ) ;
#9140 = CARTESIAN_POINT ( 'NONE',  ( -0.2556890074706391625, -7.756263830888999067, 10.00000000000000000 ) ) ;
#9141 = ADVANCED_FACE ( 'NONE', ( #10311, #5736 ), #9461, .F. ) ;
#9142 = CARTESIAN_POINT ( 'NONE',  ( -6.947552178111042309, -1.615339808524891563, 6.857782953271941950E-17 ) ) ;
#9143 = CARTESIAN_POINT ( 'NONE',  ( 3.000000000000000888, 0.000000000000000000, 0.000000000000000000 ) ) ;
#9144 = CARTESIAN_POINT ( 'NONE',  ( 3.000000000000000888, -17.97274125076083351, 13.62355943574013750 ) ) ;
#9145 = ORIENTED_EDGE ( 'NONE', *, *, #7699, .T. ) ;
#9146 = EDGE_CURVE ( 'NONE', #7842, #1170, #10702, .T. ) ;
#9147 = ORIENTED_EDGE ( 'NONE', *, *, #4216, .T. ) ;
#9148 = ORIENTED_EDGE ( 'NONE', *, *, #5873, .T. ) ;
#9149 = CARTESIAN_POINT ( 'NONE',  ( 7.972781652389874907, 11.51689705412746711, 10.00000000000000000 ) ) ;
#9150 = DIRECTION ( 'NONE',  ( -1.000000000000000000, -0.000000000000000000, 0.000000000000000000 ) ) ;
#9151 = LINE ( 'NONE', #9838, #1146 ) ;
#9152 = STYLED_ITEM ( 'NONE', ( #5059 ), #8710 ) ;
#9153 = CARTESIAN_POINT ( 'NONE',  ( -5.920784292472551336, 6.290491683487165808, 3.747395293195558847E-16 ) ) ;
#9154 = DIRECTION ( 'NONE',  ( 0.000000000000000000, 0.000000000000000000, -1.000000000000000000 ) ) ;
#9155 = LINE ( 'NONE', #6227, #9178 ) ;
#9156 = ADVANCED_FACE ( 'NONE', ( #9697 ), #5104, .T. ) ;
#9157 = ORIENTED_EDGE ( 'NONE', *, *, #11682, .T. ) ;
#9158 = ORIENTED_EDGE ( 'NONE', *, *, #6131, .T. ) ;
#9159 = ORIENTED_EDGE ( 'NONE', *, *, #5107, .T. ) ;
#9160 = CYLINDRICAL_SURFACE ( 'NONE', #3585, 9.599999999999997868 ) ;
#9161 = DIRECTION ( 'NONE',  ( -1.000000000000000000, 0.000000000000000000, 0.000000000000000000 ) ) ;
#9162 = PRODUCT_DEFINITION_CONTEXT ( 'detailed design', #2155, 'design' ) ;
#9163 = DIRECTION ( 'NONE',  ( -1.000000000000000000, 0.000000000000000000, 0.000000000000000000 ) ) ;
#9164 = EDGE_CURVE ( 'NONE', #3509, #9866, #7169, .T. ) ;
#9165 = FACE_OUTER_BOUND ( 'NONE', #8422, .T. ) ;
#9166 = CARTESIAN_POINT ( 'NONE',  ( 3.000000000000000888, 15.64281154287620446, -16.85990652506883691 ) ) ;
#9167 = DIRECTION ( 'NONE',  ( -1.000000000000000000, 0.000000000000000000, -0.000000000000000000 ) ) ;
#9168 = AXIS2_PLACEMENT_3D ( 'NONE', #3543, #11854, #10829 ) ;
#9169 = AXIS2_PLACEMENT_3D ( 'NONE', #8068, #6521, #6177 ) ;
#9170 = CARTESIAN_POINT ( 'NONE',  ( 0.000000000000000000, 0.000000000000000000, 0.000000000000000000 ) ) ;
#9171 = ORIENTED_EDGE ( 'NONE', *, *, #8948, .F. ) ;
#9172 = ORIENTED_EDGE ( 'NONE', *, *, #5274, .F. ) ;
#9173 = DIRECTION ( 'NONE',  ( 0.000000000000000000, 0.000000000000000000, -1.000000000000000000 ) ) ;
#9174 = ORIENTED_EDGE ( 'NONE', *, *, #8972, .T. ) ;
#9175 = CARTESIAN_POINT ( 'NONE',  ( -4.158289900078591117, 7.437556212722741478, 10.00000000000000000 ) ) ;
#9176 = DIRECTION ( 'NONE',  ( 0.000000000000000000, 0.000000000000000000, 1.000000000000000000 ) ) ;
#9177 = ORIENTED_EDGE ( 'NONE', *, *, #2318, .T. ) ;
#9178 = VECTOR ( 'NONE', #658, 1000.000000000000000 ) ;
#9179 = CARTESIAN_POINT ( 'NONE',  ( 0.000000000000000000, -16.45023496161654819, -15.42759117534402513 ) ) ;
#9180 = DIRECTION ( 'NONE',  ( -1.000000000000000000, -0.000000000000000000, 0.000000000000000000 ) ) ;
#9181 = CARTESIAN_POINT ( 'NONE',  ( 11.73504485001147124, -12.52947377801878837, 6.857782953271941950E-17 ) ) ;
#9182 = DIRECTION ( 'NONE',  ( -1.000000000000000000, 0.000000000000000000, 0.000000000000000000 ) ) ;
#9183 = DIRECTION ( 'NONE',  ( -1.000000000000000000, 0.000000000000000000, -0.000000000000000000 ) ) ;
#9184 = ORIENTED_EDGE ( 'NONE', *, *, #11008, .T. ) ;
#9185 = EDGE_CURVE ( 'NONE', #2061, #9879, #6014, .T. ) ;
#9186 = CARTESIAN_POINT ( 'NONE',  ( 3.000000000000000888, 0.000000000000000000, 0.000000000000000000 ) ) ;
#9187 = AXIS2_PLACEMENT_3D ( 'NONE', #9677, #4047, #4973 ) ;
#9188 = EDGE_LOOP ( 'NONE', ( #11281, #569, #3788, #9177 ) ) ;
#9189 = PRODUCT_DEFINITION_FORMATION_WITH_SPECIFIED_SOURCE ( 'ANY', '', #9411, .NOT_KNOWN. ) ;
#9190 = CARTESIAN_POINT ( 'NONE',  ( -0.9167995209625431352, 5.268308710424121521, 3.747395293195558847E-16 ) ) ;
#9191 = EDGE_CURVE ( 'NONE', #1430, #532, #6809, .T. ) ;
#9192 = CARTESIAN_POINT ( 'NONE',  ( 7.228014483236684722E-17, -0.4999999999999993339, 0.000000000000000000 ) ) ;
#9193 = VERTEX_POINT ( 'NONE', #1260 ) ;
#9194 = AXIS2_PLACEMENT_3D ( 'NONE', #381, #10544, #2163 ) ;
#9195 = FACE_OUTER_BOUND ( 'NONE', #8334, .T. ) ;
#9196 = CIRCLE ( 'NONE', #399, 9.599999999999997868 ) ;
#9197 = CIRCLE ( 'NONE', #6664, 9.599999999999997868 ) ;
#9198 = LINE ( 'NONE', #8288, #3347 ) ;
#9199 = CARTESIAN_POINT ( 'NONE',  ( 3.000000000000000888, 13.72351598154924979, -20.65684170206477788 ) ) ;
#9200 = CARTESIAN_POINT ( 'NONE',  ( 17.46093749967478814, -1.431715403549062904, 10.00000000000000000 ) ) ;
#9201 = CIRCLE ( 'NONE', #204, 9.599999999999997868 ) ;
#9202 = EDGE_CURVE ( 'NONE', #219, #1419, #6154, .T. ) ;
#9203 = CARTESIAN_POINT ( 'NONE',  ( -0.5113267480521395125, 6.289062763288773894, 6.857782953271941950E-17 ) ) ;
#9204 = PRODUCT_DEFINITION_FORMATION_WITH_SPECIFIED_SOURCE ( 'ANY', '', #18, .NOT_KNOWN. ) ;
#9205 =( LENGTH_UNIT ( ) NAMED_UNIT ( * ) SI_UNIT ( .MILLI., .METRE. ) );
#9206 = ADVANCED_FACE ( 'NONE', ( #7799 ), #5167, .T. ) ;
#9207 = DIRECTION ( 'NONE',  ( 0.000000000000000000, 0.000000000000000000, 1.000000000000000000 ) ) ;
#9208 = ORIENTED_EDGE ( 'NONE', *, *, #5032, .T. ) ;
#9209 = ADVANCED_FACE ( 'NONE', ( #7864, #6989 ), #2348, .F. ) ;
#9210 = CIRCLE ( 'NONE', #1977, 24.80000000000000071 ) ;
#9211 = VECTOR ( 'NONE', #10879, 1000.000000000000000 ) ;
#9212 = AXIS2_PLACEMENT_3D ( 'NONE', #9383, #5468, #11951 ) ;
#9213 = VERTEX_POINT ( 'NONE', #11597 ) ;
#9214 = DIRECTION ( 'NONE',  ( -0.000000000000000000, 0.000000000000000000, 1.000000000000000000 ) ) ;
#9215 = CARTESIAN_POINT ( 'NONE',  ( -6.597323627732286866, 9.514359934152452070, 10.00000000000000000 ) ) ;
#9216 = FACE_OUTER_BOUND ( 'NONE', #11512, .T. ) ;
#9217 = CARTESIAN_POINT ( 'NONE',  ( 0.000000000000000000, 0.000000000000000000, 0.000000000000000000 ) ) ;
#9218 = EDGE_CURVE ( 'NONE', #1936, #7518, #3866, .T. ) ;
#9219 = CIRCLE ( 'NONE', #9410, 24.80000000000000071 ) ;
#9220 = CARTESIAN_POINT ( 'NONE',  ( 9.640149279600553456, 4.768118462334743235, 3.747395293195558847E-16 ) ) ;
#9221 = DIRECTION ( 'NONE',  ( 0.000000000000000000, 0.000000000000000000, 1.000000000000000000 ) ) ;
#9222 = DIRECTION ( 'NONE',  ( 0.000000000000000000, 0.000000000000000000, 1.000000000000000000 ) ) ;
#9223 = ORIENTED_EDGE ( 'NONE', *, *, #7588, .T. ) ;
#9224 = CYLINDRICAL_SURFACE ( 'NONE', #8207, 24.80000000000000071 ) ;
#9225 = ORIENTED_EDGE ( 'NONE', *, *, #10555, .F. ) ;
#9226 = ORIENTED_EDGE ( 'NONE', *, *, #5180, .T. ) ;
#9227 = PRESENTATION_LAYER_ASSIGNMENT (  '', '', ( #6101 ) ) ;
#9228 = ORIENTED_EDGE ( 'NONE', *, *, #8790, .T. ) ;
#9229 = DIRECTION ( 'NONE',  ( 0.000000000000000000, -0.8660254037844328234, -0.5000000000000101030 ) ) ;
#9230 = CIRCLE ( 'NONE', #3956, 24.80000000000000071 ) ;
#9231 = CARTESIAN_POINT ( 'NONE',  ( 3.000000000000000888, 21.97817939804039611, 11.48910920600691554 ) ) ;
#9232 = DIRECTION ( 'NONE',  ( -1.000000000000000000, -0.000000000000000000, 0.000000000000000000 ) ) ;
#9233 = DIRECTION ( 'NONE',  ( -1.000000000000000000, 0.000000000000000000, 3.061616997868383141E-16 ) ) ;
#9234 = ADVANCED_FACE ( 'NONE', ( #4305 ), #11475, .T. ) ;
#9235 = CARTESIAN_POINT ( 'NONE',  ( 0.000000000000000000, -0.3433949777333296094, 22.99643626497956816 ) ) ;
#9236 = CARTESIAN_POINT ( 'NONE',  ( -7.115032382426029756, -13.85544350050026452, 3.747395293195558847E-16 ) ) ;
#9237 = CARTESIAN_POINT ( 'NONE',  ( -1.500000000000000222, 1.836970198721030181E-16, -15.00000000000000000 ) ) ;
#9238 = CIRCLE ( 'NONE', #5337, 22.99899999999999523 ) ;
#9239 = DIRECTION ( 'NONE',  ( 0.000000000000000000, 0.2079116908177532641, 0.9781476007338070211 ) ) ;
#9240 = VERTEX_POINT ( 'NONE', #11649 ) ;
#9241 = ORIENTED_EDGE ( 'NONE', *, *, #8560, .F. ) ;
#9242 = CARTESIAN_POINT ( 'NONE',  ( 3.500000000000000000, 0.000000000000000000, 1.000000000000000888 ) ) ;
#9243 = EDGE_CURVE ( 'NONE', #11379, #2984, #4056, .T. ) ;
#9244 = EDGE_LOOP ( 'NONE', ( #2150, #4144, #3980, #10559 ) ) ;
#9245 = CARTESIAN_POINT ( 'NONE',  ( -5.069009347565514467, 2.772702716245054155, 10.00000000000000000 ) ) ;
#9246 = VECTOR ( 'NONE', #3861, 1000.000000000000000 ) ;
#9247 = DIRECTION ( 'NONE',  ( 0.000000000000000000, 0.000000000000000000, 1.000000000000000000 ) ) ;
#9248 = EDGE_LOOP ( 'NONE', ( #3091, #10455, #4361, #294 ) ) ;
#9249 = AXIS2_PLACEMENT_3D ( 'NONE', #11306, #10321, #1755 ) ;
#9250 = FACE_OUTER_BOUND ( 'NONE', #2955, .T. ) ;
#9251 = AXIS2_PLACEMENT_3D ( 'NONE', #11170, #1070, #3825 ) ;
#9252 = DIRECTION ( 'NONE',  ( -1.000000000000000000, 0.000000000000000000, -0.000000000000000000 ) ) ;
#9253 = CARTESIAN_POINT ( 'NONE',  ( -5.152979166089619589, -5.321787192520355703, 10.00000000000000000 ) ) ;
#9254 = CYLINDRICAL_SURFACE ( 'NONE', #2584, 9.599999999999997868 ) ;
#9255 = CARTESIAN_POINT ( 'NONE',  ( 0.000000000000000000, 0.000000000000000000, 4.000000000000000000 ) ) ;
#9256 = AXIS2_PLACEMENT_3D ( 'NONE', #1465, #11916, #10766 ) ;
#9257 = ORIENTED_EDGE ( 'NONE', *, *, #8917, .T. ) ;
#9258 = LINE ( 'NONE', #11037, #7430 ) ;
#9259 = ORIENTED_EDGE ( 'NONE', *, *, #10289, .F. ) ;
#9260 = CARTESIAN_POINT ( 'NONE',  ( 6.841929108544086091, -2.672872603904024480, 3.747395293195558847E-16 ) ) ;
#9261 = DIRECTION ( 'NONE',  ( 0.000000000000000000, 0.000000000000000000, 1.000000000000000000 ) ) ;
#9262 = SURFACE_STYLE_FILL_AREA ( #8348 ) ;
#9263 = AXIS2_PLACEMENT_3D ( 'NONE', #2533, #2716, #6508 ) ;
#9264 = CARTESIAN_POINT ( 'NONE',  ( 0.000000000000000000, -12.88318129270191825, 18.51065745848373822 ) ) ;
#9265 = CARTESIAN_POINT ( 'NONE',  ( 3.000000000000000888, 0.000000000000000000, 0.000000000000000000 ) ) ;
#9266 = CARTESIAN_POINT ( 'NONE',  ( 17.50000000000000000, 0.000000000000000000, 10.00000000000000000 ) ) ;
#9267 = CARTESIAN_POINT ( 'NONE',  ( 1.737537816361722331, -4.672682311025833535, 6.857782953271941950E-17 ) ) ;
#9268 = CARTESIAN_POINT ( 'NONE',  ( -10.00000000000000000, 0.000000000000000000, 0.000000000000000000 ) ) ;
#9269 = CARTESIAN_POINT ( 'NONE',  ( 3.000000000000000888, 10.87771529938188486, -19.75591328264875202 ) ) ;
#9270 = EDGE_LOOP ( 'NONE', ( #6547, #3985 ) ) ;
#9271 = APPLICATION_CONTEXT ( 'automotive_design' ) ;
#9272 = EDGE_LOOP ( 'NONE', ( #3672, #3615 ) ) ;
#9273 = AXIS2_PLACEMENT_3D ( 'NONE', #1778, #9127, #9982 ) ;
#9274 = ORIENTED_EDGE ( 'NONE', *, *, #10698, .F. ) ;
#9275 = PRODUCT_DEFINITION ( 'UNKNOWN', '', #9204, #3294 ) ;
#9276 = CARTESIAN_POINT ( 'NONE',  ( 3.000000000000000888, -20.86861857134741172, 9.667200211209745930 ) ) ;
#9277 = CARTESIAN_POINT ( 'NONE',  ( 0.5199114366211746718, 8.229807867079658834, 10.00000000000000000 ) ) ;
#9278 = EDGE_CURVE ( 'NONE', #3560, #8517, #4472, .T. ) ;
#9279 = DIRECTION ( 'NONE',  ( 0.000000000000000000, 0.000000000000000000, -1.000000000000000000 ) ) ;
#9280 = CARTESIAN_POINT ( 'NONE',  ( 3.000000000000000888, -10.87771529938174808, 19.75591328264882662 ) ) ;
#9281 = EDGE_CURVE ( 'NONE', #5271, #1630, #9640, .T. ) ;
#9282 = CARTESIAN_POINT ( 'NONE',  ( 10.39479819782869541, 2.258419626871296604, 3.747395293195558847E-16 ) ) ;
#9283 = CIRCLE ( 'NONE', #1856, 9.599999999999999645 ) ;
#9284 = DIRECTION ( 'NONE',  ( 0.000000000000000000, 0.000000000000000000, 1.000000000000000000 ) ) ;
#9285 = LINE ( 'NONE', #1877, #7438 ) ;
#9286 = ORIENTED_EDGE ( 'NONE', *, *, #4723, .T. ) ;
#9287 = ORIENTED_EDGE ( 'NONE', *, *, #8826, .F. ) ;
#9288 = ORIENTED_EDGE ( 'NONE', *, *, #8405, .T. ) ;
#9289 = EDGE_CURVE ( 'NONE', #5671, #5364, #508, .T. ) ;
#9290 = DIRECTION ( 'NONE',  ( -1.000000000000000000, 0.000000000000000000, 0.000000000000000000 ) ) ;
#9291 = DIRECTION ( 'NONE',  ( -1.000000000000000000, 0.000000000000000000, 0.000000000000000000 ) ) ;
#9292 = DIRECTION ( 'NONE',  ( 0.000000000000000000, 0.000000000000000000, 1.000000000000000000 ) ) ;
#9293 = UNCERTAINTY_MEASURE_WITH_UNIT (LENGTH_MEASURE( 1.000000000000000082E-05 ), #5409, 'distance_accuracy_value', 'NONE');
#9294 = DIRECTION ( 'NONE',  ( -1.000000000000000000, 0.000000000000000000, -0.000000000000000000 ) ) ;
#9295 = FACE_OUTER_BOUND ( 'NONE', #2451, .T. ) ;
#9296 = CARTESIAN_POINT ( 'NONE',  ( 12.96212312671852551, -3.473279994529273829, 3.747395293195558847E-16 ) ) ;
#9297 = CARTESIAN_POINT ( 'NONE',  ( 1.661435237661581521, -7.700870200009177324, 6.857782953271941950E-17 ) ) ;
#9298 = EDGE_CURVE ( 'NONE', #6260, #5789, #7794, .T. ) ;
#9299 = CARTESIAN_POINT ( 'NONE',  ( 1.499999999999999556, -1.556492618230804759, 24.75110766671651774 ) ) ;
#9300 = EDGE_LOOP ( 'NONE', ( #9208, #3868, #199, #4579 ) ) ;
#9301 = ORIENTED_EDGE ( 'NONE', *, *, #8476, .T. ) ;
#9302 = DIRECTION ( 'NONE',  ( 1.000000000000000000, 0.000000000000000000, 0.000000000000000000 ) ) ;
#9303 = ORIENTED_EDGE ( 'NONE', *, *, #3898, .T. ) ;
#9304 = EDGE_CURVE ( 'NONE', #8343, #2229, #4085, .T. ) ;
#9305 = ORIENTED_EDGE ( 'NONE', *, *, #6208, .T. ) ;
#9306 = CARTESIAN_POINT ( 'NONE',  ( 0.000000000000000000, -19.29833442572351743, -11.67026512804567062 ) ) ;
#9307 = FACE_OUTER_BOUND ( 'NONE', #11077, .T. ) ;
#9308 = ADVANCED_FACE ( 'NONE', ( #7049 ), #2233, .T. ) ;
#9309 = EDGE_LOOP ( 'NONE', ( #2769, #4450 ) ) ;
#9310 = CARTESIAN_POINT ( 'NONE',  ( -10.00000000000000000, 0.000000000000000000, 0.000000000000000000 ) ) ;
#9311 = ADVANCED_FACE ( 'NONE', ( #9195 ), #8162, .T. ) ;
#9312 = DIRECTION ( 'NONE',  ( -1.000000000000000000, 0.000000000000000000, 0.000000000000000000 ) ) ;
#9313 = CARTESIAN_POINT ( 'NONE',  ( -5.101271054653079950, -15.85638610327790765, 6.857782953271941950E-17 ) ) ;
#9314 = PRODUCT_DEFINITION_SHAPE ( 'NONE', 'NONE',  #12120 ) ;
#9315 = FACE_OUTER_BOUND ( 'NONE', #2542, .T. ) ;
#9316 = VERTEX_POINT ( 'NONE', #883 ) ;
#9317 = AXIS2_PLACEMENT_3D ( 'NONE', #721, #11014, #1463 ) ;
#9318 = VERTEX_POINT ( 'NONE', #1622 ) ;
#9319 = DIRECTION ( 'NONE',  ( -1.000000000000000000, -0.000000000000000000, -0.000000000000000000 ) ) ;
#9320 = ORIENTED_EDGE ( 'NONE', *, *, #5198, .F. ) ;
#9321 = CARTESIAN_POINT ( 'NONE',  ( 1.631735293711819246, 4.895207720155139164, 3.747395293195558847E-16 ) ) ;
#9322 = DIRECTION ( 'NONE',  ( 1.000000000000000000, 0.000000000000000000, 0.000000000000000000 ) ) ;
#9323 = DIRECTION ( 'NONE',  ( -1.000000000000000000, 0.000000000000000000, 0.000000000000000000 ) ) ;
#9324 = ADVANCED_FACE ( 'NONE', ( #3461 ), #2601, .T. ) ;
#9325 = CARTESIAN_POINT ( 'NONE',  ( 3.000000000000000888, -22.54798042742717357, -0.4575788569254196636 ) ) ;
#9326 = CARTESIAN_POINT ( 'NONE',  ( 8.000000000000000000, 2.265596578422603002E-15, -18.49999999999999645 ) ) ;
#9327 = CARTESIAN_POINT ( 'NONE',  ( -6.191802569540376666, -3.848120238389427072, 6.857782953271941950E-17 ) ) ;
#9328 = DIRECTION ( 'NONE',  ( -1.000000000000000000, -0.000000000000000000, -0.000000000000000000 ) ) ;
#9329 = DIRECTION ( 'NONE',  ( -1.000000000000000000, -0.000000000000000000, 0.000000000000000000 ) ) ;
#9330 = CYLINDRICAL_SURFACE ( 'NONE', #9603, 9.599999999999997868 ) ;
#9331 = EDGE_LOOP ( 'NONE', ( #3655, #7861, #10203, #1464 ) ) ;
#9332 = ORIENTED_EDGE ( 'NONE', *, *, #2048, .F. ) ;
#9333 = VERTEX_POINT ( 'NONE', #3403 ) ;
#9334 = LINE ( 'NONE', #1866, #12094 ) ;
#9335 = CARTESIAN_POINT ( 'NONE',  ( 7.078846155420733588, 8.354583459611244933, 10.00000000000000000 ) ) ;
#9336 = DIRECTION ( 'NONE',  ( 0.000000000000000000, 0.000000000000000000, 1.000000000000000000 ) ) ;
#9337 = CARTESIAN_POINT ( 'NONE',  ( 0.000000000000000000, 0.000000000000000000, 0.000000000000000000 ) ) ;
#9338 = CARTESIAN_POINT ( 'NONE',  ( 3.000000000000000888, 0.000000000000000000, 0.000000000000000000 ) ) ;
#9339 = CARTESIAN_POINT ( 'NONE',  ( -8.984113827416486231, -1.502549133976348372, 3.747395293195558847E-16 ) ) ;
#9340 = DIRECTION ( 'NONE',  ( 1.000000000000000000, -0.000000000000000000, -0.000000000000000000 ) ) ;
#9341 = CARTESIAN_POINT ( 'NONE',  ( 0.000000000000000000, 0.000000000000000000, -15.00000000000000000 ) ) ;
#9342 = ORIENTED_EDGE ( 'NONE', *, *, #2415, .F. ) ;
#9343 = ORIENTED_EDGE ( 'NONE', *, *, #3530, .F. ) ;
#9344 = EDGE_CURVE ( 'NONE', #4720, #7859, #2917, .T. ) ;
#9345 = EDGE_LOOP ( 'NONE', ( #8249, #11637, #10599, #7072 ) ) ;
#9346 = CARTESIAN_POINT ( 'NONE',  ( 3.000000000000000888, -20.78471918669854901, -8.753070780933368766 ) ) ;
#9347 = DIRECTION ( 'NONE',  ( 1.000000000000000000, -0.000000000000000000, -0.000000000000000000 ) ) ;
#9348 = CIRCLE ( 'NONE', #4075, 24.80000000000000071 ) ;
#9349 = CARTESIAN_POINT ( 'NONE',  ( 3.000000000000000888, 0.000000000000000000, 0.000000000000000000 ) ) ;
#9350 = DIRECTION ( 'NONE',  ( -1.000000000000000000, 0.000000000000000000, 0.000000000000000000 ) ) ;
#9351 = CIRCLE ( 'NONE', #5441, 9.599999999999997868 ) ;
#9352 = CARTESIAN_POINT ( 'NONE',  ( 0.000000000000000000, -11.67026512804560134, 19.29833442572355651 ) ) ;
#9353 = CARTESIAN_POINT ( 'NONE',  ( 10.44364468045615801, 9.157203537817473205, 3.747395293195558847E-16 ) ) ;
#9354 = CARTESIAN_POINT ( 'NONE',  ( 3.913389251770639010, -3.458713887698550593, 6.857782953271941950E-17 ) ) ;
#9355 = EDGE_CURVE ( 'NONE', #1694, #1049, #8189, .T. ) ;
#9356 = EDGE_CURVE ( 'NONE', #2393, #277, #9749, .T. ) ;
#9357 = CARTESIAN_POINT ( 'NONE',  ( 0.000000000000000000, 21.97702544527767188, -6.779701584702504391 ) ) ;
#9358 = AXIS2_PLACEMENT_3D ( 'NONE', #2363, #10999, #768 ) ;
#9359 = VERTEX_POINT ( 'NONE', #5289 ) ;
#9360 = VERTEX_POINT ( 'NONE', #9996 ) ;
#9361 = CIRCLE ( 'NONE', #7762, 9.599999999999997868 ) ;
#9362 = DIRECTION ( 'NONE',  ( 1.000000000000000000, 0.000000000000000000, 0.000000000000000000 ) ) ;
#9363 = VERTEX_POINT ( 'NONE', #5358 ) ;
#9364 = VERTEX_POINT ( 'NONE', #7111 ) ;
#9365 = CARTESIAN_POINT ( 'NONE',  ( 1.499999999999999556, 21.97817939804055598, -11.48910920600660468 ) ) ;
#9366 = CARTESIAN_POINT ( 'NONE',  ( 3.000000000000000888, -16.85990652506910692, 15.64281154287591669 ) ) ;
#9367 = ORIENTED_EDGE ( 'NONE', *, *, #10888, .F. ) ;
#9368 = STYLED_ITEM ( 'NONE', ( #1477 ), #8430 ) ;
#9369 = FACE_OUTER_BOUND ( 'NONE', #10694, .T. ) ;
#9370 = CARTESIAN_POINT ( 'NONE',  ( -10.00000000000000000, 0.000000000000000000, 0.000000000000000000 ) ) ;
#9371 = CARTESIAN_POINT ( 'NONE',  ( 1.737537816361723220, -4.672682311025840640, 10.00000000000000000 ) ) ;
#9372 = DIRECTION ( 'NONE',  ( -1.000000000000000000, -0.000000000000000000, 0.000000000000000000 ) ) ;
#9373 = FACE_OUTER_BOUND ( 'NONE', #10431, .T. ) ;
#9374 = ORIENTED_EDGE ( 'NONE', *, *, #3908, .T. ) ;
#9375 = DIRECTION ( 'NONE',  ( -1.000000000000000000, 0.000000000000000000, 0.000000000000000000 ) ) ;
#9376 = ORIENTED_EDGE ( 'NONE', *, *, #3195, .T. ) ;
#9377 = CIRCLE ( 'NONE', #8786, 9.599999999999997868 ) ;
#9378 = CARTESIAN_POINT ( 'NONE',  ( 7.972781652389874907, 11.51689705412746711, 10.00000000000000000 ) ) ;
#9379 = CIRCLE ( 'NONE', #6048, 24.80000000000000071 ) ;
#9380 = DIRECTION ( 'NONE',  ( 0.000000000000000000, 0.000000000000000000, 1.000000000000000000 ) ) ;
#9381 = DIRECTION ( 'NONE',  ( 0.000000000000000000, -0.4067366430757886619, -0.9135454576426060846 ) ) ;
#9382 = CYLINDRICAL_SURFACE ( 'NONE', #11238, 9.599999999999997868 ) ;
#9383 = CARTESIAN_POINT ( 'NONE',  ( 3.000000000000000888, 8.753070780933430939, -20.78471918669851703 ) ) ;
#9384 = VECTOR ( 'NONE', #6214, 1000.000000000000000 ) ;
#9385 = ADVANCED_FACE ( 'NONE', ( #5411 ), #3636, .T. ) ;
#9386 = CARTESIAN_POINT ( 'NONE',  ( -0.8869411547437818788, -7.669649013129171244, 6.857782953271941950E-17 ) ) ;
#9387 = DIRECTION ( 'NONE',  ( -1.000000000000000000, 0.000000000000000000, -0.000000000000000000 ) ) ;
#9388 = AXIS2_PLACEMENT_3D ( 'NONE', #5428, #2620, #3599 ) ;
#9389 = DIRECTION ( 'NONE',  ( -1.000000000000000000, 0.000000000000000000, 0.000000000000000000 ) ) ;
#9390 = ORIENTED_EDGE ( 'NONE', *, *, #7340, .T. ) ;
#9391 = ADVANCED_FACE ( 'NONE', ( #10914 ), #10983, .T. ) ;
#9392 = EDGE_LOOP ( 'NONE', ( #7407, #9557 ) ) ;
#9393 = CARTESIAN_POINT ( 'NONE',  ( 1.499999999999999556, -24.02068490260616329, 6.168200451485678748 ) ) ;
#9394 = AXIS2_PLACEMENT_3D ( 'NONE', #11131, #10031, #11201 ) ;
#9395 = CARTESIAN_POINT ( 'NONE',  ( -2.487495860704070250, -9.331140650584721641, 10.00000000000000000 ) ) ;
#9396 = AXIS2_PLACEMENT_3D ( 'NONE', #5587, #11154, #878 ) ;
#9397 = DIRECTION ( 'NONE',  ( 0.000000000000000000, 0.000000000000000000, 1.000000000000000000 ) ) ;
#9398 = COLOUR_RGB ( '', 0.08235294, 0.09019608, 0.10196078) ;
#9399 = CARTESIAN_POINT ( 'NONE',  ( 5.319643049700911952, -8.526005966358411570, 3.747395293195558847E-16 ) ) ;
#9400 = CARTESIAN_POINT ( 'NONE',  ( 3.000000000000000888, 16.45023496161665122, 15.42759117534391322 ) ) ;
#9401 = CIRCLE ( 'NONE', #8233, 9.599999999999997868 ) ;
#9402 = CARTESIAN_POINT ( 'NONE',  ( 3.000000000000000888, -1.901833551798412847, 22.47229024614976822 ) ) ;
#9403 = VECTOR ( 'NONE', #1934, 1000.000000000000000 ) ;
#9404 = VERTEX_POINT ( 'NONE', #9138 ) ;
#9405 = AXIS2_PLACEMENT_3D ( 'NONE', #5628, #8198, #9362 ) ;
#9406 = VERTEX_POINT ( 'NONE', #818 ) ;
#9407 = ORIENTED_EDGE ( 'NONE', *, *, #71, .F. ) ;
#9408 = DIRECTION ( 'NONE',  ( 0.000000000000000000, -0.6691306063588644548, 0.7431448254773885820 ) ) ;
#9409 = DIRECTION ( 'NONE',  ( 1.000000000000000000, -0.000000000000000000, -0.000000000000000000 ) ) ;
#9410 = AXIS2_PLACEMENT_3D ( 'NONE', #3824, #10540, #11344 ) ;
#9411 = PRODUCT ( 'housing', 'housing', '', ( #1514 ) ) ;
#9412 = CARTESIAN_POINT ( 'NONE',  ( 1.500000000000000444, -15.40502424595158537, 19.43515443678397148 ) ) ;
#9413 = DIRECTION ( 'NONE',  ( -1.000000000000000000, 0.000000000000000000, -0.000000000000000000 ) ) ;
#9414 = CIRCLE ( 'NONE', #4142, 24.80000000000000071 ) ;
#9415 = LINE ( 'NONE', #11198, #260 ) ;
#9416 = CARTESIAN_POINT ( 'NONE',  ( -4.793139000956299967, -14.90149022103882892, 3.747395293195558847E-16 ) ) ;
#9417 = DIRECTION ( 'NONE',  ( -1.000000000000000000, 0.000000000000000000, 0.000000000000000000 ) ) ;
#9418 = CIRCLE ( 'NONE', #5716, 9.599999999999997868 ) ;
#9419 = DIRECTION ( 'NONE',  ( 0.000000000000000000, 0.6691306063588594588, -0.7431448254773932449 ) ) ;
#9420 = CARTESIAN_POINT ( 'NONE',  ( 0.000000000000000000, 0.000000000000000000, 0.000000000000000000 ) ) ;
#9421 = EDGE_CURVE ( 'NONE', #2308, #4256, #5621, .T. ) ;
#9422 = ORIENTED_EDGE ( 'NONE', *, *, #10463, .T. ) ;
#9423 = VERTEX_POINT ( 'NONE', #11044 ) ;
#9424 = CARTESIAN_POINT ( 'NONE',  ( 14.52660474336370200, -9.366294961249359119, 10.00000000000000000 ) ) ;
#9425 = ORIENTED_EDGE ( 'NONE', *, *, #9839, .T. ) ;
#9426 = DIRECTION ( 'NONE',  ( 0.000000000000000000, -0.5877852522924633671, -0.8090169943749546677 ) ) ;
#9427 = PRODUCT_DEFINITION ( 'UNKNOWN', '', #5294, #7076 ) ;
#9428 = DIRECTION ( 'NONE',  ( -1.000000000000000000, 0.000000000000000000, 0.000000000000000000 ) ) ;
#9429 = ORIENTED_EDGE ( 'NONE', *, *, #9057, .F. ) ;
#9430 = ADVANCED_FACE ( 'NONE', ( #9027 ), #6207, .T. ) ;
#9431 = CIRCLE ( 'NONE', #6889, 9.599999999999996092 ) ;
#9432 = FACE_OUTER_BOUND ( 'NONE', #2559, .T. ) ;
#9433 = CYLINDRICAL_SURFACE ( 'NONE', #2585, 9.599999999999997868 ) ;
#9434 = CARTESIAN_POINT ( 'NONE',  ( -16.00307013876014750, -1.840746716621878498, 6.857782953271941950E-17 ) ) ;
#9435 = LINE ( 'NONE', #121, #407 ) ;
#9436 = DIRECTION ( 'NONE',  ( -1.000000000000000000, 0.000000000000000000, 0.000000000000000000 ) ) ;
#9437 = ORIENTED_EDGE ( 'NONE', *, *, #969, .T. ) ;
#9438 = ORIENTED_EDGE ( 'NONE', *, *, #1301, .T. ) ;
#9439 = CARTESIAN_POINT ( 'NONE',  ( 3.000000000000000888, 18.51065745848377730, 12.88318129270185430 ) ) ;
#9440 = ORIENTED_EDGE ( 'NONE', *, *, #5345, .T. ) ;
#9441 = AXIS2_PLACEMENT_3D ( 'NONE', #6254, #9980, #1605 ) ;
#9442 = CARTESIAN_POINT ( 'NONE',  ( 16.25531780653859570, -2.690316503436296802, 10.00000000000000000 ) ) ;
#9443 = AXIS2_PLACEMENT_3D ( 'NONE', #10303, #3699, #7601 ) ;
#9444 = CARTESIAN_POINT ( 'NONE',  ( 0.000000000000000000, 17.97274125076092233, -13.62355943574001671 ) ) ;
#9445 = VERTEX_POINT ( 'NONE', #637 ) ;
#9446 = LINE ( 'NONE', #76, #5826 ) ;
#9447 = DIRECTION ( 'NONE',  ( 0.000000000000000000, 0.000000000000000000, 1.000000000000000000 ) ) ;
#9448 = CARTESIAN_POINT ( 'NONE',  ( -14.76245309360257174, 5.834016798581408203, 10.00000000000000000 ) ) ;
#9449 = CIRCLE ( 'NONE', #9832, 9.599999999999997868 ) ;
#9450 = CARTESIAN_POINT ( 'NONE',  ( 3.000000000000000888, -19.74380051311532114, -11.79560690673893042 ) ) ;
#9451 = CARTESIAN_POINT ( 'NONE',  ( -3.791520748785365491, -16.26028641251512497, 6.857782953271941950E-17 ) ) ;
#9452 = LINE ( 'NONE', #8540, #4706 ) ;
#9453 = EDGE_CURVE ( 'NONE', #5601, #1706, #11866, .T. ) ;
#9454 = ORIENTED_EDGE ( 'NONE', *, *, #6618, .F. ) ;
#9455 = DIRECTION ( 'NONE',  ( -1.000000000000000000, -0.000000000000000000, -0.000000000000000000 ) ) ;
#9456 = ORIENTED_EDGE ( 'NONE', *, *, #8279, .T. ) ;
#9457 = EDGE_CURVE ( 'NONE', #679, #9776, #9721, .T. ) ;
#9458 = AXIS2_PLACEMENT_3D ( 'NONE', #2681, #8320, #5622 ) ;
#9459 = CARTESIAN_POINT ( 'NONE',  ( 11.50000000000000178, 1.408343819019456373E-15, 4.000000000000000000 ) ) ;
#9460 = CARTESIAN_POINT ( 'NONE',  ( 6.391761267591818729, 8.940137919804724831, 10.00000000000000000 ) ) ;
#9461 = PLANE ( 'NONE',  #5061 ) ;
#9462 = CARTESIAN_POINT ( 'NONE',  ( -6.430932688512553064, -6.885836206077581068, 3.747395293195558847E-16 ) ) ;
#9463 = CARTESIAN_POINT ( 'NONE',  ( -12.27443204883033623, 3.949650873796764827, 6.857782953271941950E-17 ) ) ;
#9464 = ADVANCED_FACE ( 'NONE', ( #11097 ), #2714, .T. ) ;
#9465 = AXIS2_PLACEMENT_3D ( 'NONE', #8163, #10113, #1730 ) ;
#9466 = CARTESIAN_POINT ( 'NONE',  ( 0.000000000000000000, -22.99643626497957172, 0.3433949777330864706 ) ) ;
#9467 = VERTEX_POINT ( 'NONE', #10112 ) ;
#9468 = ORIENTED_EDGE ( 'NONE', *, *, #5353, .F. ) ;
#9469 = ORIENTED_EDGE ( 'NONE', *, *, #5924, .T. ) ;
#9470 = CARTESIAN_POINT ( 'NONE',  ( 3.000000000000000888, -8.753070780933015271, -20.78471918669869467 ) ) ;
#9471 = DIRECTION ( 'NONE',  ( -1.000000000000000000, -0.000000000000000000, 0.000000000000000000 ) ) ;
#9472 = ORIENTED_EDGE ( 'NONE', *, *, #10564, .T. ) ;
#9473 = CIRCLE ( 'NONE', #9859, 24.80000000000000071 ) ;
#9474 = DIRECTION ( 'NONE',  ( -1.000000000000000000, 0.000000000000000000, 0.000000000000000000 ) ) ;
#9475 = CYLINDRICAL_SURFACE ( 'NONE', #2702, 22.99899999999999878 ) ;
#9476 = DIRECTION ( 'NONE',  ( 0.000000000000000000, 0.000000000000000000, 1.000000000000000000 ) ) ;
#9477 = CARTESIAN_POINT ( 'NONE',  ( 16.25531780653859215, -2.690316503436295914, 3.747395293195558847E-16 ) ) ;
#9478 = DIRECTION ( 'NONE',  ( -1.000000000000000000, -0.000000000000000000, -0.000000000000000000 ) ) ;
#9479 = VERTEX_POINT ( 'NONE', #10178 ) ;
#9480 = VERTEX_POINT ( 'NONE', #1728 ) ;
#9481 = DIRECTION ( 'NONE',  ( -1.000000000000000000, 0.000000000000000000, 0.000000000000000000 ) ) ;
#9482 = CARTESIAN_POINT ( 'NONE',  ( -16.06046882360140060, -0.5196555361422392494, 10.00000000000000000 ) ) ;
#9483 = ORIENTED_EDGE ( 'NONE', *, *, #11448, .T. ) ;
#9484 = LINE ( 'NONE', #7578, #8275 ) ;
#9485 = CARTESIAN_POINT ( 'NONE',  ( 0.000000000000000000, 0.000000000000000000, -5.000000000000000000 ) ) ;
#9486 = ORIENTED_EDGE ( 'NONE', *, *, #10581, .F. ) ;
#9487 = PLANE ( 'NONE',  #11006 ) ;
#9488 = AXIS2_PLACEMENT_3D ( 'NONE', #1727, #10056, #9023 ) ;
#9489 = CARTESIAN_POINT ( 'NONE',  ( 0.000000000000000000, 0.000000000000000000, 0.000000000000000000 ) ) ;
#9490 = CARTESIAN_POINT ( 'NONE',  ( -7.327987143158983585, -11.36402271042705614, 6.857782953271941950E-17 ) ) ;
#9491 = DIRECTION ( 'NONE',  ( -1.000000000000000000, -0.000000000000000000, 0.000000000000000000 ) ) ;
#9492 = CYLINDRICAL_SURFACE ( 'NONE', #5321, 22.99899999999999878 ) ;
#9493 = ORIENTED_EDGE ( 'NONE', *, *, #5721, .F. ) ;
#9494 = ORIENTED_EDGE ( 'NONE', *, *, #2962, .F. ) ;
#9495 = DIRECTION ( 'NONE',  ( 0.000000000000000000, 0.9510565162951544194, -0.3090169943749450088 ) ) ;
#9496 = EDGE_CURVE ( 'NONE', #2749, #3541, #6507, .T. ) ;
#9497 = ORIENTED_EDGE ( 'NONE', *, *, #866, .F. ) ;
#9498 = CIRCLE ( 'NONE', #9105, 9.599999999999997868 ) ;
#9499 = EDGE_CURVE ( 'NONE', #8125, #10279, #9502, .T. ) ;
#9500 = CARTESIAN_POINT ( 'NONE',  ( -11.08238827499401680, -10.71925978067563001, 10.00000000000000000 ) ) ;
#9501 = CARTESIAN_POINT ( 'NONE',  ( 0.000000000000000000, -6.532525787310825116, -21.58580335785683246 ) ) ;
#9502 = LINE ( 'NONE', #11227, #9731 ) ;
#9503 = LINE ( 'NONE', #4919, #11423 ) ;
#9504 = CARTESIAN_POINT ( 'NONE',  ( -8.799721882313775723, 9.100398320382247164, 10.00000000000000000 ) ) ;
#9505 = AXIS2_PLACEMENT_3D ( 'NONE', #8813, #10761, #6842 ) ;
#9506 = DIRECTION ( 'NONE',  ( -1.000000000000000000, 0.000000000000000000, 0.000000000000000000 ) ) ;
#9507 = CARTESIAN_POINT ( 'NONE',  ( -14.60057116351879714, -4.165219547604622541, 3.747395293195558847E-16 ) ) ;
#9508 = EDGE_CURVE ( 'NONE', #5848, #1491, #4455, .T. ) ;
#9509 = DIRECTION ( 'NONE',  ( 1.000000000000000000, 0.000000000000000000, 0.000000000000000000 ) ) ;
#9510 = ORIENTED_EDGE ( 'NONE', *, *, #8564, .F. ) ;
#9511 = CARTESIAN_POINT ( 'NONE',  ( 3.000000000000000888, -21.96011696265495061, 5.135568396239952982 ) ) ;
#9512 = EDGE_CURVE ( 'NONE', #12091, #2865, #5433, .T. ) ;
#9513 = ORIENTED_EDGE ( 'NONE', *, *, #2639, .F. ) ;
#9514 = ORIENTED_EDGE ( 'NONE', *, *, #2734, .T. ) ;
#9515 = DIRECTION ( 'NONE',  ( -1.000000000000000000, -0.000000000000000000, -0.000000000000000000 ) ) ;
#9516 = CARTESIAN_POINT ( 'NONE',  ( 4.140589500486091090, -5.731468560951012314, 10.00000000000000000 ) ) ;
#9517 = CYLINDRICAL_SURFACE ( 'NONE', #4272, 24.80000000000000071 ) ;
#9518 = EDGE_CURVE ( 'NONE', #11239, #3932, #8949, .T. ) ;
#9519 = CARTESIAN_POINT ( 'NONE',  ( 4.138106518799270717, 8.052838533163344081, 10.00000000000000000 ) ) ;
#9520 = CARTESIAN_POINT ( 'NONE',  ( 12.50121531544688480, -6.953993600215016002, 6.857782953271941950E-17 ) ) ;
#9521 = EDGE_CURVE ( 'NONE', #992, #10871, #7963, .T. ) ;
#9522 = DIRECTION ( 'NONE',  ( -1.000000000000000000, -0.000000000000000000, -0.000000000000000000 ) ) ;
#9523 = EDGE_CURVE ( 'NONE', #6489, #2943, #9446, .T. ) ;
#9524 = ORIENTED_EDGE ( 'NONE', *, *, #4126, .F. ) ;
#9525 = EDGE_LOOP ( 'NONE', ( #5626, #4998, #11482, #3247 ) ) ;
#9526 = ORIENTED_EDGE ( 'NONE', *, *, #10878, .T. ) ;
#9527 = DIRECTION ( 'NONE',  ( -1.000000000000000000, 0.000000000000000000, 0.000000000000000000 ) ) ;
#9528 = CARTESIAN_POINT ( 'NONE',  ( 3.000000000000000888, 0.000000000000000000, 0.000000000000000000 ) ) ;
#9529 = VERTEX_POINT ( 'NONE', #6564 ) ;
#9530 = AXIS2_PLACEMENT_3D ( 'NONE', #6812, #2976, #3833 ) ;
#9531 = DIRECTION ( 'NONE',  ( 1.000000000000000000, -0.000000000000000000, -0.000000000000000000 ) ) ;
#9532 = DIRECTION ( 'NONE',  ( 0.000000000000000000, 0.000000000000000000, 1.000000000000000000 ) ) ;
#9533 = VECTOR ( 'NONE', #2156, 1000.000000000000000 ) ;
#9534 = LINE ( 'NONE', #1150, #5366 ) ;
#9535 = CARTESIAN_POINT ( 'NONE',  ( -7.594692469639082510, -9.901549393537251831, 3.747395293195558847E-16 ) ) ;
#9536 = EDGE_CURVE ( 'NONE', #1640, #9888, #4852, .T. ) ;
#9537 = CARTESIAN_POINT ( 'NONE',  ( 0.000000000000000000, -17.06259499759935139, -14.74749645580028101 ) ) ;
#9538 = ORIENTED_EDGE ( 'NONE', *, *, #10793, .T. ) ;
#9539 = VERTEX_POINT ( 'NONE', #11339 ) ;
#9540 = CARTESIAN_POINT ( 'NONE',  ( 0.000000000000000000, 0.000000000000000000, 0.000000000000000000 ) ) ;
#9541 = CARTESIAN_POINT ( 'NONE',  ( -16.00307013876015461, -1.840746716621879830, 10.00000000000000000 ) ) ;
#9542 = ORIENTED_EDGE ( 'NONE', *, *, #8378, .T. ) ;
#9543 = AXIS2_PLACEMENT_3D ( 'NONE', #3227, #1213, #8684 ) ;
#9544 = CARTESIAN_POINT ( 'NONE',  ( 3.000000000000000888, 0.000000000000000000, 0.000000000000000000 ) ) ;
#9545 = DIRECTION ( 'NONE',  ( -1.000000000000000000, 0.000000000000000000, -0.000000000000000000 ) ) ;
#9546 = EDGE_CURVE ( 'NONE', #1896, #10351, #4796, .T. ) ;
#9547 = CARTESIAN_POINT ( 'NONE',  ( 17.49999999999999645, 0.000000000000000000, 5.000000000000000000 ) ) ;
#9548 = VERTEX_POINT ( 'NONE', #7597 ) ;
#9549 = DIRECTION ( 'NONE',  ( 1.000000000000000000, 0.000000000000000000, 0.000000000000000000 ) ) ;
#9550 = CARTESIAN_POINT ( 'NONE',  ( 3.000000000000000888, 16.85990652506900389, 15.64281154287603215 ) ) ;
#9551 = CARTESIAN_POINT ( 'NONE',  ( -4.389456771235329846, 11.66511648340389051, 6.857782953271941950E-17 ) ) ;
#9552 = CIRCLE ( 'NONE', #3691, 9.599999999999996092 ) ;
#9553 = AXIS2_PLACEMENT_3D ( 'NONE', #2055, #2978, #9397 ) ;
#9554 = DIRECTION ( 'NONE',  ( 0.000000000000000000, 0.000000000000000000, 1.000000000000000000 ) ) ;
#9555 = ORIENTED_EDGE ( 'NONE', *, *, #2022, .F. ) ;
#9556 = DIRECTION ( 'NONE',  ( 0.000000000000000000, 0.000000000000000000, -1.000000000000000000 ) ) ;
#9557 = ORIENTED_EDGE ( 'NONE', *, *, #4269, .F. ) ;
#9558 = ORIENTED_EDGE ( 'NONE', *, *, #5264, .T. ) ;
#9559 = DIRECTION ( 'NONE',  ( -1.000000000000000000, -0.000000000000000000, 0.000000000000000000 ) ) ;
#9560 = ORIENTED_EDGE ( 'NONE', *, *, #9523, .F. ) ;
#9561 = CARTESIAN_POINT ( 'NONE',  ( 13.29800827116429929, 3.099979537169774257, 10.00000000000000000 ) ) ;
#9562 = AXIS2_PLACEMENT_3D ( 'NONE', #5253, #8359, #4333 ) ;
#9563 = DIRECTION ( 'NONE',  ( 0.000000000000000000, 0.000000000000000000, 1.000000000000000000 ) ) ;
#9564 = DIRECTION ( 'NONE',  ( 0.000000000000000000, 0.000000000000000000, 1.000000000000000000 ) ) ;
#9565 = DIRECTION ( 'NONE',  ( -1.000000000000000000, 0.000000000000000000, 0.000000000000000000 ) ) ;
#9566 = CARTESIAN_POINT ( 'NONE',  ( 10.54603994011899459, 5.199563424939650957, 10.00000000000000000 ) ) ;
#9567 = PRESENTATION_STYLE_ASSIGNMENT (( #7728 ) ) ;
#9568 = CARTESIAN_POINT ( 'NONE',  ( 13.68367311611256554, -8.822018488634762790, 3.747395293195558847E-16 ) ) ;
#9569 = EDGE_CURVE ( 'NONE', #3234, #11531, #4066, .T. ) ;
#9570 = CARTESIAN_POINT ( 'NONE',  ( 3.000000000000000888, 0.000000000000000000, 0.000000000000000000 ) ) ;
#9571 = VERTEX_POINT ( 'NONE', #4740 ) ;
#9572 = CARTESIAN_POINT ( 'NONE',  ( 0.000000000000000000, -11.48910920600699193, 21.97817939804034992 ) ) ;
#9573 = AXIS2_PLACEMENT_3D ( 'NONE', #4155, #11667, #11612 ) ;
#9574 = ADVANCED_FACE ( 'NONE', ( #11404 ), #2963, .T. ) ;
#9575 = VERTEX_POINT ( 'NONE', #10422 ) ;
#9576 = ORIENTED_EDGE ( 'NONE', *, *, #6796, .T. ) ;
#9577 = DIRECTION ( 'NONE',  ( -0.000000000000000000, -0.000000000000000000, -1.000000000000000000 ) ) ;
#9578 = CARTESIAN_POINT ( 'NONE',  ( -5.069009347565514467, 2.772702716245054155, 10.00000000000000000 ) ) ;
#9579 = EDGE_CURVE ( 'NONE', #8886, #3221, #740, .T. ) ;
#9580 = DIRECTION ( 'NONE',  ( 0.000000000000000000, 0.000000000000000000, -1.000000000000000000 ) ) ;
#9581 = ADVANCED_FACE ( 'NONE', ( #5780 ), #10481, .T. ) ;
#9582 = AXIS2_PLACEMENT_3D ( 'NONE', #4006, #5902, #446 ) ;
#9583 = CARTESIAN_POINT ( 'NONE',  ( 9.056240860197965148, 7.682302481599247557, 10.00000000000000000 ) ) ;
#9584 = CARTESIAN_POINT ( 'NONE',  ( -1.999398781552333526, 15.23274265415848916, 6.857782953271941950E-17 ) ) ;
#9585 = EDGE_CURVE ( 'NONE', #5072, #7710, #7577, .T. ) ;
#9586 = LINE ( 'NONE', #7870, #1957 ) ;
#9587 = EDGE_LOOP ( 'NONE', ( #3489, #4244, #1878, #11456 ) ) ;
#9588 = CIRCLE ( 'NONE', #3723, 9.599999999999997868 ) ;
#9589 = CIRCLE ( 'NONE', #10960, 9.599999999999996092 ) ;
#9590 = ORIENTED_EDGE ( 'NONE', *, *, #368, .F. ) ;
#9591 = DIRECTION ( 'NONE',  ( 0.000000000000000000, 0.000000000000000000, 1.000000000000000000 ) ) ;
#9592 = MECHANICAL_DESIGN_GEOMETRIC_PRESENTATION_REPRESENTATION (  '', ( #5483 ), #3146 ) ;
#9593 = DIRECTION ( 'NONE',  ( -1.000000000000000000, 0.000000000000000000, 0.000000000000000000 ) ) ;
#9594 = CARTESIAN_POINT ( 'NONE',  ( 3.000000000000000888, 13.62355943574019435, 17.97274125076078732 ) ) ;
#9595 = CARTESIAN_POINT ( 'NONE',  ( 16.50000000000000355, 0.000000000000000000, 10.00000000000000000 ) ) ;
#9596 = AXIS2_PLACEMENT_3D ( 'NONE', #1529, #428, #9860 ) ;
#9597 = CARTESIAN_POINT ( 'NONE',  ( 6.391761267590965190, 8.940137919805573929, 3.747395293195558847E-16 ) ) ;
#9598 = DIRECTION ( 'NONE',  ( 0.000000000000000000, -0.7431448254773999063, 0.6691306063588520203 ) ) ;
#9599 = ORIENTED_EDGE ( 'NONE', *, *, #12079, .F. ) ;
#9600 = ORIENTED_EDGE ( 'NONE', *, *, #10665, .F. ) ;
#9601 = APPLICATION_PROTOCOL_DEFINITION ( 'draft international standard', 'automotive_design', 1998, #6150 ) ;
#9602 = CARTESIAN_POINT ( 'NONE',  ( 7.014224211608842907, -15.49593329755746929, 10.00000000000000000 ) ) ;
#9603 = AXIS2_PLACEMENT_3D ( 'NONE', #7547, #10364, #6309 ) ;
#9604 = ORIENTED_EDGE ( 'NONE', *, *, #2664, .F. ) ;
#9605 = CIRCLE ( 'NONE', #5886, 24.80000000000000071 ) ;
#9606 = FACE_OUTER_BOUND ( 'NONE', #12047, .T. ) ;
#9607 = DIRECTION ( 'NONE',  ( 0.000000000000000000, 0.000000000000000000, 1.000000000000000000 ) ) ;
#9608 = AXIS2_PLACEMENT_3D ( 'NONE', #1321, #9764, #6100 ) ;
#9609 = EDGE_CURVE ( 'NONE', #8613, #11921, #6216, .T. ) ;
#9610 = CARTESIAN_POINT ( 'NONE',  ( 3.000000000000000888, 0.000000000000000000, 0.000000000000000000 ) ) ;
#9611 = EDGE_LOOP ( 'NONE', ( #11388, #4760, #7536, #9975 ) ) ;
#9612 = CARTESIAN_POINT ( 'NONE',  ( 3.000000000000000888, 22.42251312757879234, 5.117118920208566735 ) ) ;
#9613 = DIRECTION ( 'NONE',  ( -1.000000000000000000, -0.000000000000000000, -0.000000000000000000 ) ) ;
#9614 = CARTESIAN_POINT ( 'NONE',  ( -15.59049818040117152, 3.373450308083002724, 6.857782953271941950E-17 ) ) ;
#9615 = AXIS2_PLACEMENT_3D ( 'NONE', #3319, #7039, #10790 ) ;
#9616 = ORIENTED_EDGE ( 'NONE', *, *, #227, .T. ) ;
#9617 = EDGE_CURVE ( 'NONE', #9915, #3995, #11164, .T. ) ;
#9618 = CIRCLE ( 'NONE', #2378, 1.500000000000000222 ) ;
#9619 = CARTESIAN_POINT ( 'NONE',  ( 0.000000000000000000, -24.53384959170454849, -3.623565124517358793 ) ) ;
#9620 = VERTEX_POINT ( 'NONE', #2778 ) ;
#9621 = CARTESIAN_POINT ( 'NONE',  ( 0.000000000000000000, 11.79560690673899970, -19.74380051311527495 ) ) ;
#9622 = ORIENTED_EDGE ( 'NONE', *, *, #8155, .F. ) ;
#9623 = CARTESIAN_POINT ( 'NONE',  ( 1.050035089571674352, -12.78847817906846451, 10.00000000000000000 ) ) ;
#9624 = AXIS2_PLACEMENT_3D ( 'NONE', #10468, #9554, #4905 ) ;
#9625 = DIRECTION ( 'NONE',  ( -1.000000000000000000, 0.000000000000000000, -0.000000000000000000 ) ) ;
#9626 = FACE_BOUND ( 'NONE', #9890, .T. ) ;
#9627 = LINE ( 'NONE', #9685, #1074 ) ;
#9628 = CARTESIAN_POINT ( 'NONE',  ( 10.38524206949726469, 10.73010674553377797, 10.00000000000000000 ) ) ;
#9629 = DIRECTION ( 'NONE',  ( -1.000000000000000000, 0.000000000000000000, -0.000000000000000000 ) ) ;
#9630 = DIRECTION ( 'NONE',  ( -1.000000000000000000, 0.000000000000000000, -0.000000000000000000 ) ) ;
#9631 = FACE_OUTER_BOUND ( 'NONE', #10704, .T. ) ;
#9632 = VECTOR ( 'NONE', #1815, 1000.000000000000000 ) ;
#9633 = CARTESIAN_POINT ( 'NONE',  ( 3.000000000000000888, -17.35216073792428659, -17.71842311621547950 ) ) ;
#9634 = AXIS2_PLACEMENT_3D ( 'NONE', #3467, #944, #8538 ) ;
#9635 = VERTEX_POINT ( 'NONE', #7540 ) ;
#9636 = ORIENTED_EDGE ( 'NONE', *, *, #9761, .T. ) ;
#9637 = DIRECTION ( 'NONE',  ( -1.000000000000000000, -0.000000000000000000, 0.000000000000000000 ) ) ;
#9638 = CARTESIAN_POINT ( 'NONE',  ( 5.211919109253434712, 5.981019939437272726, 10.00000000000000000 ) ) ;
#9639 = VECTOR ( 'NONE', #118, 1000.000000000000000 ) ;
#9640 = LINE ( 'NONE', #7973, #9942 ) ;
#9641 = CARTESIAN_POINT ( 'NONE',  ( 8.025946968469186871, -7.769110617520879281, 10.00000000000000000 ) ) ;
#9642 = AXIS2_PLACEMENT_3D ( 'NONE', #7889, #3062, #7944 ) ;
#9643 = CARTESIAN_POINT ( 'NONE',  ( -11.98007164540816838, 10.17225797950327681, 6.857782953271941950E-17 ) ) ;
#9644 = DIRECTION ( 'NONE',  ( -1.000000000000000000, 0.000000000000000000, -0.000000000000000000 ) ) ;
#9645 = FACE_OUTER_BOUND ( 'NONE', #5334, .T. ) ;
#9646 = VERTEX_POINT ( 'NONE', #11285 ) ;
#9647 = AXIS2_PLACEMENT_3D ( 'NONE', #5020, #11446, #5880 ) ;
#9648 = EDGE_CURVE ( 'NONE', #4550, #2557, #2900, .T. ) ;
#9649 = ORIENTED_EDGE ( 'NONE', *, *, #11974, .T. ) ;
#9650 = DIRECTION ( 'NONE',  ( 0.000000000000000000, 0.6691306063588593478, -0.7431448254773931339 ) ) ;
#9651 = CARTESIAN_POINT ( 'NONE',  ( 16.50000000000000355, 0.000000000000000000, 10.00000000000000000 ) ) ;
#9652 = EDGE_CURVE ( 'NONE', #139, #6466, #1978, .T. ) ;
#9653 = CARTESIAN_POINT ( 'NONE',  ( -1.103316172498963521, -16.73802372459124044, 6.857782953271941950E-17 ) ) ;
#9654 = FACE_OUTER_BOUND ( 'NONE', #6313, .T. ) ;
#9655 = FACE_OUTER_BOUND ( 'NONE', #10938, .T. ) ;
#9656 = AXIS2_PLACEMENT_3D ( 'NONE', #2870, #4247, #8562 ) ;
#9657 = CARTESIAN_POINT ( 'NONE',  ( -1.719633853164446613, -9.543036404944416518, 3.747395293195558847E-16 ) ) ;
#9658 = EDGE_CURVE ( 'NONE', #7842, #8389, #4980, .T. ) ;
#9659 = CARTESIAN_POINT ( 'NONE',  ( 0.000000000000000000, 7.432877647175207159, 21.76479567747244204 ) ) ;
#9660 = ORIENTED_EDGE ( 'NONE', *, *, #8305, .T. ) ;
#9661 = ORIENTED_EDGE ( 'NONE', *, *, #213, .T. ) ;
#9662 = CARTESIAN_POINT ( 'NONE',  ( 10.64229886435067840, -13.41933351754447834, 10.00000000000000000 ) ) ;
#9663 = APPLICATION_CONTEXT ( 'automotive_design' ) ;
#9664 = ORIENTED_EDGE ( 'NONE', *, *, #2645, .T. ) ;
#9665 = CIRCLE ( 'NONE', #8884, 24.80000000000000071 ) ;
#9666 = LINE ( 'NONE', #6902, #2709 ) ;
#9667 = DIRECTION ( 'NONE',  ( 0.000000000000000000, 0.000000000000000000, 1.000000000000000000 ) ) ;
#9668 = CARTESIAN_POINT ( 'NONE',  ( 1.499999999999999556, 24.02068490260612776, 6.168200451485841285 ) ) ;
#9669 = VERTEX_POINT ( 'NONE', #9805 ) ;
#9670 = CARTESIAN_POINT ( 'NONE',  ( 3.000000000000000888, -18.51065745848386968, 12.88318129270172818 ) ) ;
#9671 = ADVANCED_FACE ( 'NONE', ( #437 ), #4916, .T. ) ;
#9672 = DIRECTION ( 'NONE',  ( 0.000000000000000000, -0.2079116908177664480, 0.9781476007338040235 ) ) ;
#9673 = CARTESIAN_POINT ( 'NONE',  ( -12.98359546555289334, 0.8565524458115012507, 6.857782953271941950E-17 ) ) ;
#9674 = ORIENTED_EDGE ( 'NONE', *, *, #6288, .T. ) ;
#9675 = ADVANCED_FACE ( 'NONE', ( #4179 ), #7036, .T. ) ;
#9676 = CARTESIAN_POINT ( 'NONE',  ( 3.000000000000000888, -5.117118920208326038, -22.42251312757885273 ) ) ;
#9677 = CARTESIAN_POINT ( 'NONE',  ( 3.000000000000000888, 0.000000000000000000, 0.000000000000000000 ) ) ;
#9678 = ORIENTED_EDGE ( 'NONE', *, *, #609, .T. ) ;
#9679 = CARTESIAN_POINT ( 'NONE',  ( 4.583115687978493114, -8.898851689027766909, 10.00000000000000000 ) ) ;
#9680 = DIRECTION ( 'NONE',  ( -1.000000000000000000, 0.000000000000000000, 0.000000000000000000 ) ) ;
#9681 = VECTOR ( 'NONE', #7045, 1000.000000000000000 ) ;
#9682 = FILL_AREA_STYLE_COLOUR ( '', #11731 ) ;
#9683 = EDGE_CURVE ( 'NONE', #2943, #4581, #10710, .T. ) ;
#9684 = FACE_OUTER_BOUND ( 'NONE', #250, .T. ) ;
#9685 = CARTESIAN_POINT ( 'NONE',  ( 1.500000000000000444, -6.168200451485581048, -24.02068490260619171 ) ) ;
#9686 = CARTESIAN_POINT ( 'NONE',  ( -7.327987143158986250, -11.36402271042610224, 10.00000000000000000 ) ) ;
#9687 =( NAMED_UNIT ( * ) PLANE_ANGLE_UNIT ( ) SI_UNIT ( $, .RADIAN. ) );
#9688 = CARTESIAN_POINT ( 'NONE',  ( 12.88139461472923841, -9.891864711284155121, 3.747395293195558847E-16 ) ) ;
#9689 = CARTESIAN_POINT ( 'NONE',  ( -3.500000000000000000, 4.286263797015736595E-16, 10.00000000000000000 ) ) ;
#9690 = CIRCLE ( 'NONE', #4412, 22.99899999999999523 ) ;
#9691 = ORIENTED_EDGE ( 'NONE', *, *, #2282, .T. ) ;
#9692 = CARTESIAN_POINT ( 'NONE',  ( 0.000000000000000000, 0.000000000000000000, 0.000000000000000000 ) ) ;
#9693 = ORIENTED_EDGE ( 'NONE', *, *, #5367, .F. ) ;
#9694 = VERTEX_POINT ( 'NONE', #5089 ) ;
#9695 = DIRECTION ( 'NONE',  ( 0.000000000000000000, -0.4067366430757887730, -0.9135454576426059736 ) ) ;
#9696 = ADVANCED_FACE ( 'NONE', ( #257 ), #9739, .T. ) ;
#9697 = FACE_OUTER_BOUND ( 'NONE', #3539, .T. ) ;
#9698 = CIRCLE ( 'NONE', #9891, 22.99900000000000233 ) ;
#9699 = LINE ( 'NONE', #2412, #10187 ) ;
#9700 = CARTESIAN_POINT ( 'NONE',  ( 3.343943643650761022, -10.41127694127790271, 10.00000000000000000 ) ) ;
#9701 = CARTESIAN_POINT ( 'NONE',  ( -8.211874628637438889, -10.69266484962706087, 6.857782953271941950E-17 ) ) ;
#9702 = LINE ( 'NONE', #10441, #6640 ) ;
#9703 = ORIENTED_EDGE ( 'NONE', *, *, #10475, .F. ) ;
#9704 = ORIENTED_EDGE ( 'NONE', *, *, #4862, .T. ) ;
#9705 = AXIS2_PLACEMENT_3D ( 'NONE', #9547, #2757, #2942 ) ;
#9706 = ORIENTED_EDGE ( 'NONE', *, *, #1724, .F. ) ;
#9707 = DIRECTION ( 'NONE',  ( -1.000000000000000000, 0.000000000000000000, 0.000000000000000000 ) ) ;
#9708 = DIRECTION ( 'NONE',  ( 0.000000000000000000, 0.000000000000000000, -1.000000000000000000 ) ) ;
#9709 = DIRECTION ( 'NONE',  ( -0.000000000000000000, 0.000000000000000000, 1.000000000000000000 ) ) ;
#9710 = DIRECTION ( 'NONE',  ( -1.000000000000000000, -0.000000000000000000, -0.000000000000000000 ) ) ;
#9711 = CARTESIAN_POINT ( 'NONE',  ( 9.962304844536467030, 3.945508033568876360, 3.747395293195558847E-16 ) ) ;
#9712 = EDGE_CURVE ( 'NONE', #348, #3644, #10904, .T. ) ;
#9713 = FACE_OUTER_BOUND ( 'NONE', #6869, .T. ) ;
#9714 = EDGE_LOOP ( 'NONE', ( #7161, #1141, #1413, #9927 ) ) ;
#9715 = ORIENTED_EDGE ( 'NONE', *, *, #6284, .F. ) ;
#9716 = APPLICATION_PROTOCOL_DEFINITION ( 'draft international standard', 'automotive_design', 1998, #8009 ) ;
#9717 = CARTESIAN_POINT ( 'NONE',  ( -12.06849956494803600, -5.462025159505909500, 10.00000000000000000 ) ) ;
#9718 = ORIENTED_EDGE ( 'NONE', *, *, #1828, .T. ) ;
#9719 = DIRECTION ( 'NONE',  ( -1.000000000000000000, 0.000000000000000000, 0.000000000000000000 ) ) ;
#9720 = LINE ( 'NONE', #5940, #7491 ) ;
#9721 = CIRCLE ( 'NONE', #4445, 9.599999999999997868 ) ;
#9722 = DIRECTION ( 'NONE',  ( 1.000000000000000000, -0.000000000000000000, -0.000000000000000000 ) ) ;
#9723 = ORIENTED_EDGE ( 'NONE', *, *, #11915, .T. ) ;
#9724 = ADVANCED_FACE ( 'NONE', ( #7724 ), #3083, .T. ) ;
#9725 = DIRECTION ( 'NONE',  ( 0.000000000000000000, 0.000000000000000000, 1.000000000000000000 ) ) ;
#9726 = EDGE_CURVE ( 'NONE', #11027, #5571, #10719, .T. ) ;
#9727 = CARTESIAN_POINT ( 'NONE',  ( 0.000000000000000000, -21.97702544527753332, -6.779701584702958250 ) ) ;
#9728 = CARTESIAN_POINT ( 'NONE',  ( 5.027256439335598515, -9.798587832408038878, 6.857782953271941950E-17 ) ) ;
#9729 = ORIENTED_EDGE ( 'NONE', *, *, #288, .F. ) ;
#9730 = DIRECTION ( 'NONE',  ( -1.000000000000000000, 0.000000000000000000, 0.000000000000000000 ) ) ;
#9731 = VECTOR ( 'NONE', #9323, 1000.000000000000000 ) ;
#9732 = ORIENTED_EDGE ( 'NONE', *, *, #11625, .T. ) ;
#9733 = CARTESIAN_POINT ( 'NONE',  ( 0.000000000000000000, -2.811977935937933104, 22.37663021667342989 ) ) ;
#9734 = VERTEX_POINT ( 'NONE', #6920 ) ;
#9735 = CARTESIAN_POINT ( 'NONE',  ( -7.402161455537875412, -5.702533393948235663, 10.00000000000000000 ) ) ;
#9736 = DIRECTION ( 'NONE',  ( -1.000000000000000000, -0.000000000000000000, 0.000000000000000000 ) ) ;
#9737 = SURFACE_STYLE_FILL_AREA ( #10663 ) ;
#9738 = AXIS2_PLACEMENT_3D ( 'NONE', #1886, #2869, #6474 ) ;
#9739 = CYLINDRICAL_SURFACE ( 'NONE', #4253, 24.80000000000000071 ) ;
#9740 = CARTESIAN_POINT ( 'NONE',  ( 0.000000000000000000, 0.000000000000000000, 0.000000000000000000 ) ) ;
#9741 = CARTESIAN_POINT ( 'NONE',  ( 10.63538685525201188, -4.008487272325480966, 10.00000000000000000 ) ) ;
#9742 = CARTESIAN_POINT ( 'NONE',  ( 3.000000000000000888, -17.31945870441157354, 15.13242714128113775 ) ) ;
#9743 = CARTESIAN_POINT ( 'NONE',  ( 16.25531780653859215, -2.690316503436295914, 3.747395293195558847E-16 ) ) ;
#9744 = CARTESIAN_POINT ( 'NONE',  ( -10.00000000000000000, 0.000000000000000000, 0.000000000000000000 ) ) ;
#9745 = ORIENTED_EDGE ( 'NONE', *, *, #11527, .F. ) ;
#9746 = CARTESIAN_POINT ( 'NONE',  ( -20.00000000000000000, 2.449293598294706513E-15, -5.000000000000000000 ) ) ;
#9747 = ORIENTED_EDGE ( 'NONE', *, *, #5161, .T. ) ;
#9748 = CIRCLE ( 'NONE', #1931, 22.99899999999999878 ) ;
#9749 = CIRCLE ( 'NONE', #11317, 22.99900000000000233 ) ;
#9750 = CARTESIAN_POINT ( 'NONE',  ( 3.500000000000000000, 0.000000000000000000, 0.000000000000000000 ) ) ;
#9751 = EDGE_CURVE ( 'NONE', #1049, #5811, #3875, .T. ) ;
#9752 = DIRECTION ( 'NONE',  ( -1.000000000000000000, 0.000000000000000000, -0.000000000000000000 ) ) ;
#9753 = ORIENTED_EDGE ( 'NONE', *, *, #5158, .F. ) ;
#9754 = CARTESIAN_POINT ( 'NONE',  ( 3.000000000000000888, 0.000000000000000000, 0.000000000000000000 ) ) ;
#9755 = CARTESIAN_POINT ( 'NONE',  ( -5.965338750500730924, 7.524205049158505965, 10.00000000000000000 ) ) ;
#9756 = CIRCLE ( 'NONE', #4880, 22.99899999999999523 ) ;
#9757 = CARTESIAN_POINT ( 'NONE',  ( -10.84705874452746066, 6.751620637727320684, 6.857782953271941950E-17 ) ) ;
#9758 = FILL_AREA_STYLE ('',( #4196 ) ) ;
#9759 = DIRECTION ( 'NONE',  ( 0.000000000000000000, 0.000000000000000000, 1.000000000000000000 ) ) ;
#9760 = ORIENTED_EDGE ( 'NONE', *, *, #6357, .F. ) ;
#9761 = EDGE_CURVE ( 'NONE', #1309, #8897, #7784, .T. ) ;
#9762 = ORIENTED_EDGE ( 'NONE', *, *, #4154, .T. ) ;
#9763 = VERTEX_POINT ( 'NONE', #315 ) ;
#9764 = DIRECTION ( 'NONE',  ( -1.000000000000000000, 0.000000000000000000, 0.000000000000000000 ) ) ;
#9765 = CIRCLE ( 'NONE', #8802, 9.599999999999997868 ) ;
#9766 = CARTESIAN_POINT ( 'NONE',  ( 1.500000000000000444, -3.623565124516942237, -24.53384959170461599 ) ) ;
#9767 = DIRECTION ( 'NONE',  ( 0.000000000000000000, 0.000000000000000000, 1.000000000000000000 ) ) ;
#9768 = CARTESIAN_POINT ( 'NONE',  ( 10.50580257846853982, 1.391709641844861123, 3.747395293195558847E-16 ) ) ;
#9769 = AXIS2_PLACEMENT_3D ( 'NONE', #335, #2114, #6884 ) ;
#9770 = CARTESIAN_POINT ( 'NONE',  ( 1.499999999999999556, -24.53384959170460178, 3.623565124517029279 ) ) ;
#9771 = VECTOR ( 'NONE', #7772, 1000.000000000000000 ) ;
#9772 = FACE_OUTER_BOUND ( 'NONE', #3816, .T. ) ;
#9773 = ORIENTED_EDGE ( 'NONE', *, *, #2846, .T. ) ;
#9774 = ORIENTED_EDGE ( 'NONE', *, *, #4040, .T. ) ;
#9775 = CARTESIAN_POINT ( 'NONE',  ( 13.06601448280975220, -5.920767845834314258, 10.00000000000000000 ) ) ;
#9776 = VERTEX_POINT ( 'NONE', #10604 ) ;
#9777 = DIRECTION ( 'NONE',  ( 0.000000000000000000, -0.9510565162951503115, -0.3090169943749572767 ) ) ;
#9778 = CARTESIAN_POINT ( 'NONE',  ( 3.000000000000000888, 21.76479567747241717, 7.432877647175279101 ) ) ;
#9779 = CIRCLE ( 'NONE', #4896, 1.500000000000000222 ) ;
#9780 = UNCERTAINTY_MEASURE_WITH_UNIT (LENGTH_MEASURE( 1.000000000000000082E-05 ), #5031, 'distance_accuracy_value', 'NONE');
#9781 = DIRECTION ( 'NONE',  ( 0.000000000000000000, 0.000000000000000000, 1.000000000000000000 ) ) ;
#9782 = AXIS2_PLACEMENT_3D ( 'NONE', #5568, #11862, #2685 ) ;
#9783 = ORIENTED_EDGE ( 'NONE', *, *, #2630, .T. ) ;
#9784 = AXIS2_PLACEMENT_3D ( 'NONE', #6792, #2149, #366 ) ;
#9785 = CARTESIAN_POINT ( 'NONE',  ( 3.000000000000000888, -9.039786367038701087, -21.14796121233205284 ) ) ;
#9786 = STYLED_ITEM ( 'NONE', ( #3253 ), #2941 ) ;
#9787 = DIRECTION ( 'NONE',  ( 0.000000000000000000, 0.000000000000000000, 1.000000000000000000 ) ) ;
#9788 = CARTESIAN_POINT ( 'NONE',  ( 7.252227276001472767, 5.017415995114415495, 6.857782953271941950E-17 ) ) ;
#9789 = EDGE_CURVE ( 'NONE', #6735, #11676, #10508, .T. ) ;
#9790 = ORIENTED_EDGE ( 'NONE', *, *, #11659, .F. ) ;
#9791 = AXIS2_PLACEMENT_3D ( 'NONE', #2952, #8761, #2146 ) ;
#9792 = DIRECTION ( 'NONE',  ( 0.000000000000000000, 0.8660254037844397068, -0.4999999999999980016 ) ) ;
#9793 = CIRCLE ( 'NONE', #5498, 24.80000000000000071 ) ;
#9794 = DIRECTION ( 'NONE',  ( -1.000000000000000000, 0.000000000000000000, -0.000000000000000000 ) ) ;
#9795 = VECTOR ( 'NONE', #8079, 1000.000000000000000 ) ;
#9796 = VERTEX_POINT ( 'NONE', #6975 ) ;
#9797 = CARTESIAN_POINT ( 'NONE',  ( -12.04643853703213807, -0.2059847383341459892, 10.00000000000000000 ) ) ;
#9798 = ADVANCED_FACE ( 'NONE', ( #9626, #1246 ), #3314, .T. ) ;
#9799 = ORIENTED_EDGE ( 'NONE', *, *, #11523, .T. ) ;
#9800 = CARTESIAN_POINT ( 'NONE',  ( 3.000000000000000888, 21.76479567747252020, -7.432877647174977120 ) ) ;
#9801 =( NAMED_UNIT ( * ) PLANE_ANGLE_UNIT ( ) SI_UNIT ( $, .RADIAN. ) );
#9802 = EDGE_LOOP ( 'NONE', ( #8341, #12117, #12006, #9847 ) ) ;
#9803 = EDGE_CURVE ( 'NONE', #11729, #10656, #12068, .T. ) ;
#9804 = CIRCLE ( 'NONE', #1987, 20.00000000000000000 ) ;
#9805 = CARTESIAN_POINT ( 'NONE',  ( 0.000000000000000000, 21.97817939804055598, -11.48910920600660646 ) ) ;
#9806 = AXIS2_PLACEMENT_3D ( 'NONE', #2661, #8229, #3522 ) ;
#9807 = DIRECTION ( 'NONE',  ( -1.000000000000000000, -0.000000000000000000, -0.000000000000000000 ) ) ;
#9808 = CARTESIAN_POINT ( 'NONE',  ( -8.665663522307777811, -5.581295667939715877, 10.00000000000000000 ) ) ;
#9809 = CARTESIAN_POINT ( 'NONE',  ( 0.000000000000000000, -17.97274125076064877, -13.62355943574037731 ) ) ;
#9810 = CARTESIAN_POINT ( 'NONE',  ( 11.72652038055309731, 7.297668919379284524, 3.747395293195558847E-16 ) ) ;
#9811 = DIRECTION ( 'NONE',  ( 1.000000000000000000, 0.000000000000000000, 0.000000000000000000 ) ) ;
#9812 = EDGE_LOOP ( 'NONE', ( #151, #6282, #8804, #2837 ) ) ;
#9813 = CARTESIAN_POINT ( 'NONE',  ( 0.000000000000000000, 0.000000000000000000, 0.000000000000000000 ) ) ;
#9814 = CIRCLE ( 'NONE', #10796, 9.599999999999996092 ) ;
#9815 = ORIENTED_EDGE ( 'NONE', *, *, #9134, .T. ) ;
#9816 = ADVANCED_FACE ( 'NONE', ( #9684 ), #1298, .F. ) ;
#9817 = CIRCLE ( 'NONE', #10798, 22.99899999999999878 ) ;
#9818 = CARTESIAN_POINT ( 'NONE',  ( 0.000000000000000000, 0.000000000000000000, 0.000000000000000000 ) ) ;
#9819 = VERTEX_POINT ( 'NONE', #2276 ) ;
#9820 = CARTESIAN_POINT ( 'NONE',  ( -10.00000000000000000, 0.000000000000000000, 0.000000000000000000 ) ) ;
#9821 = DIRECTION ( 'NONE',  ( -0.000000000000000000, -0.000000000000000000, 1.000000000000000000 ) ) ;
#9822 = CARTESIAN_POINT ( 'NONE',  ( 1.737537816361723220, -4.672682311025840640, 10.00000000000000000 ) ) ;
#9823 = AXIS2_PLACEMENT_3D ( 'NONE', #1876, #958, #4694 ) ;
#9824 = EDGE_CURVE ( 'NONE', #2472, #3273, #8090, .T. ) ;
#9825 = CARTESIAN_POINT ( 'NONE',  ( 5.835571643920552276, -9.386589068694823013, 6.857782953271941950E-17 ) ) ;
#9826 = CARTESIAN_POINT ( 'NONE',  ( 3.000000000000000888, 0.000000000000000000, 0.000000000000000000 ) ) ;
#9827 = DIRECTION ( 'NONE',  ( 0.000000000000000000, 0.000000000000000000, 1.000000000000000000 ) ) ;
#9828 = ORIENTED_EDGE ( 'NONE', *, *, #11105, .F. ) ;
#9829 = EDGE_CURVE ( 'NONE', #6927, #7251, #3383, .T. ) ;
#9830 = ORIENTED_EDGE ( 'NONE', *, *, #3456, .T. ) ;
#9831 = ORIENTED_EDGE ( 'NONE', *, *, #9121, .T. ) ;
#9832 = AXIS2_PLACEMENT_3D ( 'NONE', #1229, #9549, #4901 ) ;
#9833 = EDGE_CURVE ( 'NONE', #9318, #9844, #10314, .T. ) ;
#9834 = CARTESIAN_POINT ( 'NONE',  ( 2.839002905302877799, -15.63284973865751049, 10.00000000000000000 ) ) ;
#9835 = CIRCLE ( 'NONE', #253, 3.500000000000000000 ) ;
#9836 = CARTESIAN_POINT ( 'NONE',  ( -10.00000000000000000, 0.000000000000000000, 0.000000000000000000 ) ) ;
#9837 = CIRCLE ( 'NONE', #7084, 24.80000000000000071 ) ;
#9838 = CARTESIAN_POINT ( 'NONE',  ( 1.499999999999999556, 4.135161237383580435, 24.45282072769602166 ) ) ;
#9839 = EDGE_CURVE ( 'NONE', #10975, #9118, #1536, .T. ) ;
#9840 = CARTESIAN_POINT ( 'NONE',  ( 5.211919109253432936, 5.981019939437269173, 3.747395293195558847E-16 ) ) ;
#9841 = CIRCLE ( 'NONE', #11791, 9.599999999999997868 ) ;
#9842 = CYLINDRICAL_SURFACE ( 'NONE', #210, 22.99899999999999878 ) ;
#9843 = CARTESIAN_POINT ( 'NONE',  ( 0.000000000000000000, 4.445336973060856955, 22.56530478845650123 ) ) ;
#9844 = VERTEX_POINT ( 'NONE', #11758 ) ;
#9845 = VERTEX_POINT ( 'NONE', #6321 ) ;
#9846 = CARTESIAN_POINT ( 'NONE',  ( 4.451863640886955409, 11.26298505921346305, 10.00000000000000000 ) ) ;
#9847 = ORIENTED_EDGE ( 'NONE', *, *, #11442, .T. ) ;
#9848 = CARTESIAN_POINT ( 'NONE',  ( 0.000000000000000000, 0.000000000000000000, 0.000000000000000000 ) ) ;
#9849 = DIRECTION ( 'NONE',  ( -1.000000000000000000, 0.000000000000000000, 0.000000000000000000 ) ) ;
#9850 = CARTESIAN_POINT ( 'NONE',  ( 3.000000000000000888, -3.623565124516938685, -24.53384959170461244 ) ) ;
#9851 = ADVANCED_FACE ( 'NONE', ( #3622 ), #8945, .T. ) ;
#9852 = AXIS2_PLACEMENT_3D ( 'NONE', #1554, #3519, #9997 ) ;
#9853 = DIRECTION ( 'NONE',  ( -1.000000000000000000, -0.000000000000000000, -0.000000000000000000 ) ) ;
#9854 = ORIENTED_EDGE ( 'NONE', *, *, #4424, .F. ) ;
#9855 = CARTESIAN_POINT ( 'NONE',  ( 0.000000000000000000, 20.41249101028211754, 9.589108953447965433 ) ) ;
#9856 = DIRECTION ( 'NONE',  ( -1.000000000000000000, -0.000000000000000000, 0.000000000000000000 ) ) ;
#9857 = CARTESIAN_POINT ( 'NONE',  ( -7.130211940009568927, -7.605417807865418212, 6.857782953271941950E-17 ) ) ;
#9858 = DIRECTION ( 'NONE',  ( -1.000000000000000000, 0.000000000000000000, -0.000000000000000000 ) ) ;
#9859 = AXIS2_PLACEMENT_3D ( 'NONE', #7850, #11586, #10666 ) ;
#9860 = DIRECTION ( 'NONE',  ( 0.000000000000000000, 0.000000000000000000, 1.000000000000000000 ) ) ;
#9861 = ORIENTED_EDGE ( 'NONE', *, *, #9499, .T. ) ;
#9862 = CARTESIAN_POINT ( 'NONE',  ( -5.008276813248565773, -11.55791719732261669, 10.00000000000000000 ) ) ;
#9863 = VERTEX_POINT ( 'NONE', #5450 ) ;
#9864 = CARTESIAN_POINT ( 'NONE',  ( 3.000000000000000888, 0.000000000000000000, 0.000000000000000000 ) ) ;
#9865 = FILL_AREA_STYLE_COLOUR ( '', #6243 ) ;
#9866 = VERTEX_POINT ( 'NONE', #2698 ) ;
#9867 = DIRECTION ( 'NONE',  ( -0.000000000000000000, -0.000000000000000000, -1.000000000000000000 ) ) ;
#9868 = DIRECTION ( 'NONE',  ( -1.000000000000000000, 0.000000000000000000, -0.000000000000000000 ) ) ;
#9869 = CARTESIAN_POINT ( 'NONE',  ( 7.605204090344414247, 4.385345779697003010, 10.00000000000000000 ) ) ;
#9870 = DIRECTION ( 'NONE',  ( 0.000000000000000000, -0.3090169943749545012, 0.9510565162951513107 ) ) ;
#9871 = CARTESIAN_POINT ( 'NONE',  ( -11.32214898804403802, 3.633524203738173419, 3.747395293195558847E-16 ) ) ;
#9872 = EDGE_CURVE ( 'NONE', #3560, #10686, #10901, .T. ) ;
#9873 = CARTESIAN_POINT ( 'NONE',  ( 0.000000000000000000, -23.05871956130116018, -9.128825345753257992 ) ) ;
#9874 = EDGE_CURVE ( 'NONE', #10068, #1657, #2498, .T. ) ;
#9875 = CARTESIAN_POINT ( 'NONE',  ( 3.000000000000000888, -0.3433949777333296094, 22.99643626497956816 ) ) ;
#9876 = ORIENTED_EDGE ( 'NONE', *, *, #7929, .T. ) ;
#9877 = DIRECTION ( 'NONE',  ( -1.000000000000000000, 0.000000000000000000, 0.000000000000000000 ) ) ;
#9878 =( NAMED_UNIT ( * ) PLANE_ANGLE_UNIT ( ) SI_UNIT ( $, .RADIAN. ) );
#9879 = VERTEX_POINT ( 'NONE', #1663 ) ;
#9880 = DIRECTION ( 'NONE',  ( -1.000000000000000000, -0.000000000000000000, -0.000000000000000000 ) ) ;
#9881 = CARTESIAN_POINT ( 'NONE',  ( -3.500000000000000000, 4.286263797015736595E-16, 0.000000000000000000 ) ) ;
#9882 = CARTESIAN_POINT ( 'NONE',  ( -4.859750766525547050, 4.557676925202722273, 10.00000000000000000 ) ) ;
#9883 = ADVANCED_FACE ( 'NONE', ( #5273 ), #11998, .T. ) ;
#9884 = CARTESIAN_POINT ( 'NONE',  ( -8.799721882313772170, 9.100398320382241835, 6.857782953271941950E-17 ) ) ;
#9885 = SURFACE_STYLE_FILL_AREA ( #10807 ) ;
#9886 = EDGE_CURVE ( 'NONE', #7518, #9078, #251, .T. ) ;
#9887 = DIRECTION ( 'NONE',  ( -1.000000000000000000, 0.000000000000000000, 0.000000000000000000 ) ) ;
#9888 = VERTEX_POINT ( 'NONE', #2456 ) ;
#9889 = ORIENTED_EDGE ( 'NONE', *, *, #2846, .F. ) ;
#9890 = EDGE_LOOP ( 'NONE', ( #9706, #6239 ) ) ;
#9891 = AXIS2_PLACEMENT_3D ( 'NONE', #4848, #128, #3024 ) ;
#9892 = CARTESIAN_POINT ( 'NONE',  ( 7.983652613117085295, -10.39416588708253997, 10.00000000000000000 ) ) ;
#9893 = CARTESIAN_POINT ( 'NONE',  ( 0.000000000000000000, 22.56530478845649057, 4.445336973060936891 ) ) ;
#9894 = DIRECTION ( 'NONE',  ( 0.000000000000000000, -6.866613759074863256E-15, 1.000000000000000000 ) ) ;
#9895 = CARTESIAN_POINT ( 'NONE',  ( -5.319913005755192437, -3.351504787100450855, 3.747395293195558847E-16 ) ) ;
#9896 = CARTESIAN_POINT ( 'NONE',  ( 1.500000000000000444, 17.71842311621552923, -17.35216073792423330 ) ) ;
#9897 = AXIS2_PLACEMENT_3D ( 'NONE', #9610, #1226, #9781 ) ;
#9898 = DIRECTION ( 'NONE',  ( -1.000000000000000000, -0.000000000000000000, -0.000000000000000000 ) ) ;
#9899 = ORIENTED_EDGE ( 'NONE', *, *, #6168, .T. ) ;
#9900 = ORIENTED_EDGE ( 'NONE', *, *, #1644, .F. ) ;
#9901 = CARTESIAN_POINT ( 'NONE',  ( -12.27443204882852257, 3.949650873796767492, 10.00000000000000000 ) ) ;
#9902 = ORIENTED_EDGE ( 'NONE', *, *, #10856, .T. ) ;
#9903 = CARTESIAN_POINT ( 'NONE',  ( 4.525508228541173850, -0.2388087992699347017, 10.00000000000000000 ) ) ;
#9904 = CYLINDRICAL_SURFACE ( 'NONE', #10340, 9.599999999999997868 ) ;
#9905 = DIRECTION ( 'NONE',  ( -1.000000000000000000, 0.000000000000000000, -0.000000000000000000 ) ) ;
#9906 = CARTESIAN_POINT ( 'NONE',  ( 3.000000000000000888, -4.240409074144249502, 22.15038895030647836 ) ) ;
#9907 = ORIENTED_EDGE ( 'NONE', *, *, #6655, .T. ) ;
#9908 = EDGE_CURVE ( 'NONE', #4202, #8369, #10416, .T. ) ;
#9909 = CARTESIAN_POINT ( 'NONE',  ( 3.000000000000000888, 22.15038895030649257, 4.240409074144170454 ) ) ;
#9910 = DIRECTION ( 'NONE',  ( -1.000000000000000000, 0.000000000000000000, 0.000000000000000000 ) ) ;
#9911 = CARTESIAN_POINT ( 'NONE',  ( -6.506554845699739076, -8.196137552275128968, 6.857782953271941950E-17 ) ) ;
#9912 = DIRECTION ( 'NONE',  ( 1.000000000000000000, 0.000000000000000000, 0.000000000000000000 ) ) ;
#9913 = CARTESIAN_POINT ( 'NONE',  ( 3.000000000000000888, -0.3433949777333296094, 22.99643626497956816 ) ) ;
#9914 = EDGE_CURVE ( 'NONE', #2253, #1383, #8072, .T. ) ;
#9915 = VERTEX_POINT ( 'NONE', #801 ) ;
#9916 = CARTESIAN_POINT ( 'NONE',  ( -0.1586286459269548865, 8.284426055182342097, 10.00000000000000000 ) ) ;
#9917 = VERTEX_POINT ( 'NONE', #6195 ) ;
#9918 = DIRECTION ( 'NONE',  ( 0.000000000000000000, -0.4067366430757888285, -0.9135454576426059736 ) ) ;
#9919 = DIRECTION ( 'NONE',  ( -1.000000000000000000, -0.000000000000000000, -0.000000000000000000 ) ) ;
#9920 = DIRECTION ( 'NONE',  ( -1.000000000000000000, -0.000000000000000000, -0.000000000000000000 ) ) ;
#9921 = DIRECTION ( 'NONE',  ( 0.000000000000000000, -0.2079116908177468526, -0.9781476007338083534 ) ) ;
#9922 = CARTESIAN_POINT ( 'NONE',  ( 10.96671743108979058, -3.132869264233008266, 10.00000000000000000 ) ) ;
#9923 = DIRECTION ( 'NONE',  ( 0.000000000000000000, -0.1045284632676607012, 0.9945218953682726237 ) ) ;
#9924 = CARTESIAN_POINT ( 'NONE',  ( 9.683839015878911383, 10.01260560230520547, 3.747395293195558847E-16 ) ) ;
#9925 = CARTESIAN_POINT ( 'NONE',  ( 3.000000000000000888, -2.062268319295719632, 22.90635393027945454 ) ) ;
#9926 = LINE ( 'NONE', #9875, #4709 ) ;
#9927 = ORIENTED_EDGE ( 'NONE', *, *, #3739, .T. ) ;
#9928 = FACE_OUTER_BOUND ( 'NONE', #4819, .T. ) ;
#9929 = VECTOR ( 'NONE', #4150, 1000.000000000000000 ) ;
#9930 = CIRCLE ( 'NONE', #5242, 9.599999999999996092 ) ;
#9931 = CARTESIAN_POINT ( 'NONE',  ( 3.000000000000000888, -20.78471918669854901, -8.753070780933368766 ) ) ;
#9932 = ORIENTED_EDGE ( 'NONE', *, *, #1715, .F. ) ;
#9933 = CARTESIAN_POINT ( 'NONE',  ( -10.00000000000000000, 0.000000000000000000, 0.000000000000000000 ) ) ;
#9934 = CARTESIAN_POINT ( 'NONE',  ( 0.000000000000000000, 0.000000000000000000, 0.000000000000000000 ) ) ;
#9935 = DIRECTION ( 'NONE',  ( 1.000000000000000000, -0.000000000000000000, 0.000000000000000000 ) ) ;
#9936 = CARTESIAN_POINT ( 'NONE',  ( 11.50231346626665285, 1.508968394323198847, 6.857782953271941950E-17 ) ) ;
#9937 = CARTESIAN_POINT ( 'NONE',  ( 0.000000000000000000, -15.42759117534397006, 16.45023496161660148 ) ) ;
#9938 = AXIS2_PLACEMENT_3D ( 'NONE', #1744, #4631, #6524 ) ;
#9939 = CARTESIAN_POINT ( 'NONE',  ( 0.000000000000000000, -3.623565124517270419, 24.53384959170456270 ) ) ;
#9940 = ADVANCED_FACE ( 'NONE', ( #4354 ), #736, .T. ) ;
#9941 = ORIENTED_EDGE ( 'NONE', *, *, #6830, .T. ) ;
#9942 = VECTOR ( 'NONE', #11708, 1000.000000000000000 ) ;
#9943 = VERTEX_POINT ( 'NONE', #5341 ) ;
#9944 = EDGE_LOOP ( 'NONE', ( #385, #11716, #6751, #2298 ) ) ;
#9945 = EDGE_CURVE ( 'NONE', #11132, #1751, #6699, .T. ) ;
#9946 = CARTESIAN_POINT ( 'NONE',  ( -11.15100792855599110, -5.055838994807845488, 10.00000000000000000 ) ) ;
#9947 = EDGE_CURVE ( 'NONE', #5671, #2749, #11786, .T. ) ;
#9948 = AXIS2_PLACEMENT_3D ( 'NONE', #7447, #8020, #10843 ) ;
#9949 = CARTESIAN_POINT ( 'NONE',  ( 0.000000000000000000, 21.58580335785685378, -6.532525787310757615 ) ) ;
#9950 = DIRECTION ( 'NONE',  ( 0.000000000000000000, -0.7431448254773863615, -0.6691306063588672304 ) ) ;
#9951 = EDGE_CURVE ( 'NONE', #219, #10824, #5348, .T. ) ;
#9952 = CARTESIAN_POINT ( 'NONE',  ( -5.846204292276366843, 1.022993486932169516, 3.747395293195558847E-16 ) ) ;
#9953 = DIRECTION ( 'NONE',  ( 0.000000000000000000, 0.000000000000000000, 1.000000000000000000 ) ) ;
#9954 = CARTESIAN_POINT ( 'NONE',  ( 0.000000000000000000, -15.42759117534374447, -16.45023496161680754 ) ) ;
#9955 = AXIS2_PLACEMENT_3D ( 'NONE', #5804, #4022, #1147 ) ;
#9956 = VERTEX_POINT ( 'NONE', #8208 ) ;
#9957 = ORIENTED_EDGE ( 'NONE', *, *, #2250, .F. ) ;
#9958 = AXIS2_PLACEMENT_3D ( 'NONE', #1096, #11491, #9598 ) ;
#9959 = VERTEX_POINT ( 'NONE', #11028 ) ;
#9960 = CARTESIAN_POINT ( 'NONE',  ( 0.5697670706242778937, -3.781298318517896551, 10.00000000000000000 ) ) ;
#9961 = CARTESIAN_POINT ( 'NONE',  ( 3.000000000000000888, 19.29833442572375546, -11.67026512804527272 ) ) ;
#9962 = CYLINDRICAL_SURFACE ( 'NONE', #1528, 9.599999999999997868 ) ;
#9963 = ORIENTED_EDGE ( 'NONE', *, *, #9872, .F. ) ;
#9964 = CARTESIAN_POINT ( 'NONE',  ( 3.000000000000000888, -17.06259499759954679, 14.74749645580005364 ) ) ;
#9965 = AXIS2_PLACEMENT_3D ( 'NONE', #8543, #2673, #7549 ) ;
#9966 = CARTESIAN_POINT ( 'NONE',  ( 3.000000000000000888, 21.14796121233209192, -9.039786367038628256 ) ) ;
#9967 = CARTESIAN_POINT ( 'NONE',  ( 4.764169229608189227, 7.652272242164855243, 6.857782953271941950E-17 ) ) ;
#9968 = ADVANCED_FACE ( 'NONE', ( #4544 ), #8274, .T. ) ;
#9969 = DIRECTION ( 'NONE',  ( 0.000000000000000000, 0.3090169943749479509, -0.9510565162951534202 ) ) ;
#9970 = ORIENTED_EDGE ( 'NONE', *, *, #6755, .F. ) ;
#9971 = FACE_OUTER_BOUND ( 'NONE', #10924, .T. ) ;
#9972 = AXIS2_PLACEMENT_3D ( 'NONE', #6926, #5842, #7790 ) ;
#9973 = EDGE_LOOP ( 'NONE', ( #761, #4698 ) ) ;
#9974 = ADVANCED_FACE ( 'NONE', ( #5763 ), #11325, .T. ) ;
#9975 = ORIENTED_EDGE ( 'NONE', *, *, #9951, .T. ) ;
#9976 = AXIS2_PLACEMENT_3D ( 'NONE', #7264, #8325, #3729 ) ;
#9977 = CARTESIAN_POINT ( 'NONE',  ( 5.892341078160698409, -4.186101517074010125, 10.00000000000000000 ) ) ;
#9978 = CIRCLE ( 'NONE', #9187, 24.80000000000000071 ) ;
#9979 = DIRECTION ( 'NONE',  ( -1.000000000000000000, 0.000000000000000000, -0.000000000000000000 ) ) ;
#9980 = DIRECTION ( 'NONE',  ( -1.000000000000000000, 0.000000000000000000, 0.000000000000000000 ) ) ;
#9981 = EDGE_CURVE ( 'NONE', #8199, #6260, #10341, .T. ) ;
#9982 = DIRECTION ( 'NONE',  ( 0.000000000000000000, 0.1045284632676471287, 0.9945218953682740670 ) ) ;
#9983 = CARTESIAN_POINT ( 'NONE',  ( -3.909826107003197215, 8.641065831729468627, 10.00000000000000000 ) ) ;
#9984 = CIRCLE ( 'NONE', #3938, 24.80000000000000071 ) ;
#9985 = VECTOR ( 'NONE', #3782, 1000.000000000000000 ) ;
#9986 = CARTESIAN_POINT ( 'NONE',  ( 3.500000000000000000, 0.000000000000000000, -15.00000000000000000 ) ) ;
#9987 = LINE ( 'NONE', #3449, #586 ) ;
#9988 = ORIENTED_EDGE ( 'NONE', *, *, #633, .F. ) ;
#9989 = DIRECTION ( 'NONE',  ( 0.000000000000000000, 0.000000000000000000, 1.000000000000000000 ) ) ;
#9990 = VERTEX_POINT ( 'NONE', #2945 ) ;
#9991 = CARTESIAN_POINT ( 'NONE',  ( -4.491015865170908228, 3.510096388331549910, 3.747395293195558847E-16 ) ) ;
#9992 = CIRCLE ( 'NONE', #10359, 22.99899999999999523 ) ;
#9993 = DIRECTION ( 'NONE',  ( -0.000000000000000000, -0.000000000000000000, -1.000000000000000000 ) ) ;
#9994 = VERTEX_POINT ( 'NONE', #60 ) ;
#9995 = AXIS2_PLACEMENT_3D ( 'NONE', #5687, #10740, #47 ) ;
#9996 = CARTESIAN_POINT ( 'NONE',  ( 3.000000000000000888, 19.10918332567978695, -15.80756504416672215 ) ) ;
#9997 = DIRECTION ( 'NONE',  ( 1.000000000000000000, 0.000000000000000000, 0.000000000000000000 ) ) ;
#9998 = CARTESIAN_POINT ( 'NONE',  ( 0.0002901587068752367257, -4.749354241797645315, 10.00000000000000000 ) ) ;
#9999 = CARTESIAN_POINT ( 'NONE',  ( 4.451863640887384399, 11.26298505921345594, 6.857782953271941950E-17 ) ) ;
#10000 = CARTESIAN_POINT ( 'NONE',  ( 3.000000000000000888, 24.77821629063821973, 1.039229259764575364 ) ) ;
#10001 = AXIS2_PLACEMENT_3D ( 'NONE', #4666, #8398, #3746 ) ;
#10002 = DIRECTION ( 'NONE',  ( -1.000000000000000000, 0.000000000000000000, -0.000000000000000000 ) ) ;
#10003 = ORIENTED_EDGE ( 'NONE', *, *, #1272, .F. ) ;
#10004 = CIRCLE ( 'NONE', #11575, 20.00000000000000000 ) ;
#10005 = ORIENTED_EDGE ( 'NONE', *, *, #7162, .F. ) ;
#10006 = CARTESIAN_POINT ( 'NONE',  ( 13.03626601087043113, 4.193914020169875911, 10.00000000000000000 ) ) ;
#10007 = AXIS2_PLACEMENT_3D ( 'NONE', #6785, #3068, #4221 ) ;
#10008 = DIRECTION ( 'NONE',  ( -0.000000000000000000, -0.000000000000000000, 1.000000000000000000 ) ) ;
#10009 = DIRECTION ( 'NONE',  ( -0.07332096784667033185, -0.9973083954695395326, 0.000000000000000000 ) ) ;
#10010 = CARTESIAN_POINT ( 'NONE',  ( -2.214925388403154116, 4.996014981202573146, 3.747395293195558847E-16 ) ) ;
#10011 = LINE ( 'NONE', #7305, #9211 ) ;
#10012 = ADVANCED_FACE ( 'NONE', ( #9250 ), #6607, .T. ) ;
#10013 = CARTESIAN_POINT ( 'NONE',  ( 1.500000000000000444, -23.24434456306319419, -8.645255683529244450 ) ) ;
#10014 = ORIENTED_EDGE ( 'NONE', *, *, #4192, .F. ) ;
#10015 = ORIENTED_EDGE ( 'NONE', *, *, #2465, .F. ) ;
#10016 = PRODUCT_CONTEXT ( 'NONE', #5124, 'mechanical' ) ;
#10017 = ADVANCED_FACE ( 'NONE', ( #9432 ), #11271, .T. ) ;
#10018 = ORIENTED_EDGE ( 'NONE', *, *, #6624, .F. ) ;
#10019 = CARTESIAN_POINT ( 'NONE',  ( -0.4771094043438766641, 5.286185534804332065, 10.00000000000000000 ) ) ;
#10020 = AXIS2_PLACEMENT_3D ( 'NONE', #4721, #5698, #9426 ) ;
#10021 = DIRECTION ( 'NONE',  ( 0.000000000000000000, 0.000000000000000000, 1.000000000000000000 ) ) ;
#10022 = UNCERTAINTY_MEASURE_WITH_UNIT (LENGTH_MEASURE( 1.000000000000000082E-05 ), #1330, 'distance_accuracy_value', 'NONE');
#10023 = FACE_OUTER_BOUND ( 'NONE', #8899, .T. ) ;
#10024 = ORIENTED_EDGE ( 'NONE', *, *, #6762, .F. ) ;
#10025 = AXIS2_PLACEMENT_3D ( 'NONE', #6434, #1902, #8576 ) ;
#10026 = DIRECTION ( 'NONE',  ( 0.000000000000000000, 0.000000000000000000, 1.000000000000000000 ) ) ;
#10027 = CARTESIAN_POINT ( 'NONE',  ( 3.000000000000000888, -10.87771529938148518, -19.75591328264897228 ) ) ;
#10028 = CARTESIAN_POINT ( 'NONE',  ( 8.539395351299290837, 0.2748098766782898217, 6.857782953271941950E-17 ) ) ;
#10029 = ADVANCED_FACE ( 'NONE', ( #9369 ), #870, .T. ) ;
#10030 = AXIS2_PLACEMENT_3D ( 'NONE', #6724, #11267, #4833 ) ;
#10031 = DIRECTION ( 'NONE',  ( -1.000000000000000000, -0.000000000000000000, 0.000000000000000000 ) ) ;
#10032 = ORIENTED_EDGE ( 'NONE', *, *, #8781, .F. ) ;
#10033 = DIRECTION ( 'NONE',  ( -1.000000000000000000, 0.000000000000000000, 0.000000000000000000 ) ) ;
#10034 = ORIENTED_EDGE ( 'NONE', *, *, #10417, .F. ) ;
#10035 = CIRCLE ( 'NONE', #854, 9.599999999999999645 ) ;
#10036 = ORIENTED_EDGE ( 'NONE', *, *, #9726, .T. ) ;
#10037 = CARTESIAN_POINT ( 'NONE',  ( -8.111627617515260624, 3.498804908652024093, 10.00000000000000000 ) ) ;
#10038 = VERTEX_POINT ( 'NONE', #10406 ) ;
#10039 = ADVANCED_FACE ( 'NONE', ( #4603 ), #9487, .T. ) ;
#10040 = CARTESIAN_POINT ( 'NONE',  ( 3.000000000000000888, 0.000000000000000000, 0.000000000000000000 ) ) ;
#10041 = ORIENTED_EDGE ( 'NONE', *, *, #10692, .T. ) ;
#10042 = DIRECTION ( 'NONE',  ( -1.000000000000000000, 0.000000000000000000, 0.000000000000000000 ) ) ;
#10043 = CARTESIAN_POINT ( 'NONE',  ( 3.000000000000000888, -7.402892494506152943, -21.30300407174369681 ) ) ;
#10044 = CARTESIAN_POINT ( 'NONE',  ( -3.764233030011072678, -6.516208816467838894, 10.00000000000000000 ) ) ;
#10045 = EDGE_CURVE ( 'NONE', #7806, #6896, #2023, .T. ) ;
#10046 = CIRCLE ( 'NONE', #4972, 22.99900000000000588 ) ;
#10047 = CARTESIAN_POINT ( 'NONE',  ( 3.000000000000000888, 1.556492618230968628, -24.75110766671650353 ) ) ;
#10048 = DIRECTION ( 'NONE',  ( 0.000000000000000000, -6.866613759074863256E-15, 1.000000000000000000 ) ) ;
#10049 = ORIENTED_EDGE ( 'NONE', *, *, #11369, .F. ) ;
#10050 = ORIENTED_EDGE ( 'NONE', *, *, #4814, .F. ) ;
#10051 = CARTESIAN_POINT ( 'NONE',  ( 3.000000000000000888, -19.43515443678392529, -15.40502424595165110 ) ) ;
#10052 = EDGE_LOOP ( 'NONE', ( #7769, #11412, #10683, #6530 ) ) ;
#10053 = EDGE_CURVE ( 'NONE', #5516, #8808, #4166, .T. ) ;
#10054 = CARTESIAN_POINT ( 'NONE',  ( -3.231136241382283725, -5.666136714102345984, 3.747395293195558847E-16 ) ) ;
#10055 = VECTOR ( 'NONE', #5958, 1000.000000000000000 ) ;
#10056 = DIRECTION ( 'NONE',  ( -1.000000000000000000, -0.000000000000000000, 0.000000000000000000 ) ) ;
#10057 = EDGE_LOOP ( 'NONE', ( #6251, #1187, #2971, #5222 ) ) ;
#10058 = DIRECTION ( 'NONE',  ( -1.000000000000000000, 0.000000000000000000, -0.000000000000000000 ) ) ;
#10059 = DIRECTION ( 'NONE',  ( -1.000000000000000000, 0.000000000000000000, 0.000000000000000000 ) ) ;
#10060 = CARTESIAN_POINT ( 'NONE',  ( 4.698850784960275639, -6.565226861933597391, 10.00000000000000000 ) ) ;
#10061 = EDGE_CURVE ( 'NONE', #11676, #10279, #5138, .T. ) ;
#10062 = CARTESIAN_POINT ( 'NONE',  ( -1.032305814202111760, 6.265050879046235366, 6.857782953271941950E-17 ) ) ;
#10063 = DIRECTION ( 'NONE',  ( -1.000000000000000000, -0.000000000000000000, -0.000000000000000000 ) ) ;
#10064 = CYLINDRICAL_SURFACE ( 'NONE', #983, 9.599999999999996092 ) ;
#10065 = ORIENTED_EDGE ( 'NONE', *, *, #6475, .F. ) ;
#10066 = VERTEX_POINT ( 'NONE', #5579 ) ;
#10067 = ADVANCED_FACE ( 'NONE', ( #8335 ), #12056, .F. ) ;
#10068 = VERTEX_POINT ( 'NONE', #7401 ) ;
#10069 = CARTESIAN_POINT ( 'NONE',  ( 13.53515989517831919, -0.2218654272303337005, 10.00000000000000000 ) ) ;
#10070 = CARTESIAN_POINT ( 'NONE',  ( 3.000000000000000888, 16.85990652506920995, -15.64281154287580655 ) ) ;
#10071 = CARTESIAN_POINT ( 'NONE',  ( 3.000000000000000888, 0.000000000000000000, 0.000000000000000000 ) ) ;
#10072 = CIRCLE ( 'NONE', #7132, 9.599999999999999645 ) ;
#10073 = CARTESIAN_POINT ( 'NONE',  ( -0.7379871813790714885, -6.677365878963852808, 3.747395293195558847E-16 ) ) ;
#10074 = CARTESIAN_POINT ( 'NONE',  ( 3.000000000000000888, 0.000000000000000000, 0.000000000000000000 ) ) ;
#10075 = DIRECTION ( 'NONE',  ( -1.000000000000000000, -0.000000000000000000, -0.000000000000000000 ) ) ;
#10076 = ORIENTED_EDGE ( 'NONE', *, *, #1115, .T. ) ;
#10077 = VERTEX_POINT ( 'NONE', #924 ) ;
#10078 = ORIENTED_EDGE ( 'NONE', *, *, #11320, .T. ) ;
#10079 = CARTESIAN_POINT ( 'NONE',  ( 3.006682760306614632, 4.002877712838978752, 10.00000000000000000 ) ) ;
#10080 = DIRECTION ( 'NONE',  ( 0.000000000000000000, 0.9510565162951523099, 0.3090169943749513370 ) ) ;
#10081 = FACE_OUTER_BOUND ( 'NONE', #7120, .T. ) ;
#10082 = CARTESIAN_POINT ( 'NONE',  ( -19.99999999999999645, 0.000000000000000000, 0.000000000000000000 ) ) ;
#10083 = VECTOR ( 'NONE', #6906, 1000.000000000000000 ) ;
#10084 = EDGE_CURVE ( 'NONE', #8696, #9118, #2611, .T. ) ;
#10085 = DIRECTION ( 'NONE',  ( 1.000000000000000000, -0.000000000000000000, -0.000000000000000000 ) ) ;
#10086 = CARTESIAN_POINT ( 'NONE',  ( -6.947552178111042309, -1.615339808524891563, 6.857782953271941950E-17 ) ) ;
#10087 = DIRECTION ( 'NONE',  ( -1.000000000000000000, 0.000000000000000000, 0.000000000000000000 ) ) ;
#10088 = EDGE_LOOP ( 'NONE', ( #7222, #1072, #4297, #10981 ) ) ;
#10089 = LINE ( 'NONE', #4654, #1588 ) ;
#10090 = ORIENTED_EDGE ( 'NONE', *, *, #9585, .F. ) ;
#10091 = ORIENTED_EDGE ( 'NONE', *, *, #1492, .F. ) ;
#10092 = CARTESIAN_POINT ( 'NONE',  ( -1.515734900794040829, 8.225284064336937817, 10.00000000000000000 ) ) ;
#10093 = EDGE_CURVE ( 'NONE', #10640, #5406, #2995, .T. ) ;
#10094 = EDGE_LOOP ( 'NONE', ( #3133, #8968, #2238, #2031 ) ) ;
#10095 = FACE_OUTER_BOUND ( 'NONE', #5137, .T. ) ;
#10096 = EDGE_LOOP ( 'NONE', ( #8644, #8497, #235, #3305 ) ) ;
#10097 = EDGE_CURVE ( 'NONE', #5247, #10333, #7271, .T. ) ;
#10098 = CARTESIAN_POINT ( 'NONE',  ( 3.000000000000000888, 5.135568396240338451, -21.96011696265485824 ) ) ;
#10099 = ADVANCED_FACE ( 'NONE', ( #11213 ), #4727, .T. ) ;
#10100 = LINE ( 'NONE', #871, #7706 ) ;
#10101 = CARTESIAN_POINT ( 'NONE',  ( 5.508953106497951779, 1.454581011951755043, 10.00000000000000000 ) ) ;
#10102 =( NAMED_UNIT ( * ) SI_UNIT ( $, .STERADIAN. ) SOLID_ANGLE_UNIT ( ) );
#10103 = CYLINDRICAL_SURFACE ( 'NONE', #1388, 22.99899999999999878 ) ;
#10104 = ORIENTED_EDGE ( 'NONE', *, *, #11527, .T. ) ;
#10105 = ORIENTED_EDGE ( 'NONE', *, *, #11812, .T. ) ;
#10106 = DIRECTION ( 'NONE',  ( -1.000000000000000000, 0.000000000000000000, -0.000000000000000000 ) ) ;
#10107 = VERTEX_POINT ( 'NONE', #6908 ) ;
#10108 = EDGE_CURVE ( 'NONE', #9571, #762, #6784, .T. ) ;
#10109 = CARTESIAN_POINT ( 'NONE',  ( 16.46093749971205966, -1.349437486485980386, 10.00000000000000000 ) ) ;
#10110 = CARTESIAN_POINT ( 'NONE',  ( 0.000000000000000000, -22.37663021667341923, 6.788022064061986605 ) ) ;
#10111 = AXIS2_PLACEMENT_3D ( 'NONE', #2840, #2042, #7482 ) ;
#10112 = CARTESIAN_POINT ( 'NONE',  ( 0.000000000000000000, 6.168200451485757796, 24.02068490260614908 ) ) ;
#10113 = DIRECTION ( 'NONE',  ( -1.000000000000000000, 0.000000000000000000, -0.000000000000000000 ) ) ;
#10114 = CARTESIAN_POINT ( 'NONE',  ( -11.98007164540817371, 10.17225797950328214, 10.00000000000000000 ) ) ;
#10115 = CARTESIAN_POINT ( 'NONE',  ( 3.666996827460249797, 4.772409917195337137, 6.857782953271941950E-17 ) ) ;
#10116 = FACE_OUTER_BOUND ( 'NONE', #4651, .T. ) ;
#10117 = DIRECTION ( 'NONE',  ( -1.000000000000000000, 0.000000000000000000, -0.000000000000000000 ) ) ;
#10118 = ORIENTED_EDGE ( 'NONE', *, *, #1982, .T. ) ;
#10119 = AXIS2_PLACEMENT_3D ( 'NONE', #222, #9710, #9532 ) ;
#10120 = VERTEX_POINT ( 'NONE', #2140 ) ;
#10121 = ORIENTED_EDGE ( 'NONE', *, *, #4485, .T. ) ;
#10122 = EDGE_CURVE ( 'NONE', #9694, #4337, #9449, .T. ) ;
#10123 = DIRECTION ( 'NONE',  ( 0.000000000000000000, 0.000000000000000000, 1.000000000000000000 ) ) ;
#10124 = CARTESIAN_POINT ( 'NONE',  ( -3.516813791735897254, 7.717845097288996037, 10.00000000000000000 ) ) ;
#10125 = CARTESIAN_POINT ( 'NONE',  ( 0.000000000000000000, -11.20082935824061110, -20.08719549084876732 ) ) ;
#10126 = CARTESIAN_POINT ( 'NONE',  ( 3.000000000000000888, -13.79477846460783574, -18.40266524480602683 ) ) ;
#10127 = CARTESIAN_POINT ( 'NONE',  ( -4.158289900079266133, 7.437556212723415605, 3.747395293195558847E-16 ) ) ;
#10128 = AXIS2_PLACEMENT_3D ( 'NONE', #9280, #7302, #1871 ) ;
#10129 = AXIS2_PLACEMENT_3D ( 'NONE', #2548, #12024, #7431 ) ;
#10130 = EDGE_CURVE ( 'NONE', #3750, #10107, #6511, .T. ) ;
#10131 = DIRECTION ( 'NONE',  ( 1.000000000000000000, 0.000000000000000000, 0.000000000000000000 ) ) ;
#10132 = DIRECTION ( 'NONE',  ( 0.000000000000000000, 0.000000000000000000, 1.000000000000000000 ) ) ;
#10133 = ORIENTED_EDGE ( 'NONE', *, *, #8254, .T. ) ;
#10134 = DIRECTION ( 'NONE',  ( -1.000000000000000000, 0.000000000000000000, 0.000000000000000000 ) ) ;
#10135 = EDGE_LOOP ( 'NONE', ( #2359, #6375, #5954, #3354 ) ) ;
#10136 = ORIENTED_EDGE ( 'NONE', *, *, #10575, .F. ) ;
#10137 = CARTESIAN_POINT ( 'NONE',  ( 0.000000000000000000, -18.40266524480598065, 13.79477846460790502 ) ) ;
#10138 = AXIS2_PLACEMENT_3D ( 'NONE', #1691, #9041, #9098 ) ;
#10139 = CARTESIAN_POINT ( 'NONE',  ( 3.000000000000000888, -20.08719549084872824, 11.20082935824068038 ) ) ;
#10140 = DIRECTION ( 'NONE',  ( 0.000000000000000000, -0.1045284632676401204, -0.9945218953682746221 ) ) ;
#10141 = UNCERTAINTY_MEASURE_WITH_UNIT (LENGTH_MEASURE( 1.000000000000000082E-05 ), #1001, 'distance_accuracy_value', 'NONE');
#10142 = CARTESIAN_POINT ( 'NONE',  ( 0.000000000000000000, -24.02068490260616329, 6.168200451485676972 ) ) ;
#10143 = DIRECTION ( 'NONE',  ( -1.000000000000000000, -0.000000000000000000, -0.000000000000000000 ) ) ;
#10144 = CARTESIAN_POINT ( 'NONE',  ( 0.000000000000000000, 0.000000000000000000, 0.000000000000000000 ) ) ;
#10145 = CARTESIAN_POINT ( 'NONE',  ( 3.000000000000000888, -13.23915371906942440, -18.80635025205183197 ) ) ;
#10146 = CIRCLE ( 'NONE', #10928, 9.599999999999996092 ) ;
#10147 = VECTOR ( 'NONE', #6135, 1000.000000000000000 ) ;
#10148 = CIRCLE ( 'NONE', #11130, 9.599999999999997868 ) ;
#10149 = CARTESIAN_POINT ( 'NONE',  ( 3.000000000000000888, 22.83456483164692585, -2.745295967525759995 ) ) ;
#10150 = ORIENTED_EDGE ( 'NONE', *, *, #10951, .T. ) ;
#10151 = ORIENTED_EDGE ( 'NONE', *, *, #4649, .T. ) ;
#10152 = CARTESIAN_POINT ( 'NONE',  ( 1.500000000000000444, 17.35216073792464897, -17.71842311621511712 ) ) ;
#10153 = EDGE_LOOP ( 'NONE', ( #9889, #7819 ) ) ;
#10154 = ORIENTED_EDGE ( 'NONE', *, *, #2406, .T. ) ;
#10155 = CIRCLE ( 'NONE', #11718, 3.500000000000000000 ) ;
#10156 = CARTESIAN_POINT ( 'NONE',  ( -4.428608208598376450, -4.627450663479480752, 10.00000000000000000 ) ) ;
#10157 = ORIENTED_EDGE ( 'NONE', *, *, #6208, .F. ) ;
#10158 = DIRECTION ( 'NONE',  ( 0.000000000000000000, 0.000000000000000000, 1.000000000000000000 ) ) ;
#10159 = EDGE_LOOP ( 'NONE', ( #7459, #3772, #1172, #7891 ) ) ;
#10160 = AXIS2_PLACEMENT_3D ( 'NONE', #3089, #5788, #6928 ) ;
#10161 = ADVANCED_FACE ( 'NONE', ( #3126 ), #8703, .T. ) ;
#10162 = CARTESIAN_POINT ( 'NONE',  ( 0.000000000000000000, 0.000000000000000000, 0.000000000000000000 ) ) ;
#10163 = CARTESIAN_POINT ( 'NONE',  ( 3.000000000000000888, -9.589108953448036488, 20.41249101028208202 ) ) ;
#10164 = CARTESIAN_POINT ( 'NONE',  ( 4.503282398431824873, -2.806195971666264111, 10.00000000000000000 ) ) ;
#10165 = VECTOR ( 'NONE', #10117, 1000.000000000000000 ) ;
#10166 = CARTESIAN_POINT ( 'NONE',  ( 3.000000000000000888, 8.753070780933159156, 20.78471918669863427 ) ) ;
#10167 = VERTEX_POINT ( 'NONE', #4219 ) ;
#10168 = VERTEX_POINT ( 'NONE', #5819 ) ;
#10169 = CARTESIAN_POINT ( 'NONE',  ( -10.00000000000000000, 0.000000000000000000, 0.000000000000000000 ) ) ;
#10170 = EDGE_CURVE ( 'NONE', #3469, #6885, #9055, .T. ) ;
#10171 = AXIS2_PLACEMENT_3D ( 'NONE', #10294, #3629, #11280 ) ;
#10172 = ORIENTED_EDGE ( 'NONE', *, *, #8756, .F. ) ;
#10173 = EDGE_CURVE ( 'NONE', #139, #4299, #7680, .T. ) ;
#10174 = CARTESIAN_POINT ( 'NONE',  ( 5.498207398720008854, -4.630339417915828371, 3.747395293195558847E-16 ) ) ;
#10175 = CARTESIAN_POINT ( 'NONE',  ( -3.000000000000000000, 3.673940397442059868E-16, -15.00000000000000000 ) ) ;
#10176 = FILL_AREA_STYLE_COLOUR ( '', #10374 ) ;
#10177 = AXIS2_PLACEMENT_3D ( 'NONE', #7102, #10726, #2462 ) ;
#10178 = CARTESIAN_POINT ( 'NONE',  ( 0.000000000000000000, -21.97817939804031795, -11.48910920600707186 ) ) ;
#10179 = AXIS2_PLACEMENT_3D ( 'NONE', #5510, #6368, #2751 ) ;
#10180 = CARTESIAN_POINT ( 'NONE',  ( 0.000000000000000000, 0.000000000000000000, 0.000000000000000000 ) ) ;
#10181 = CARTESIAN_POINT ( 'NONE',  ( 11.73504485001147835, -12.52947377801879192, 10.00000000000000000 ) ) ;
#10182 = CARTESIAN_POINT ( 'NONE',  ( 4.503282398433332112, -2.806195971666638922, 6.857782953271941950E-17 ) ) ;
#10183 = CARTESIAN_POINT ( 'NONE',  ( 0.000000000000000000, 0.000000000000000000, 0.000000000000000000 ) ) ;
#10184 = EDGE_CURVE ( 'NONE', #9575, #8512, #2403, .T. ) ;
#10185 = FACE_OUTER_BOUND ( 'NONE', #2333, .T. ) ;
#10186 = VERTEX_POINT ( 'NONE', #1340 ) ;
#10187 = VECTOR ( 'NONE', #4933, 1000.000000000000000 ) ;
#10188 = VECTOR ( 'NONE', #7067, 1000.000000000000000 ) ;
#10189 = AXIS2_PLACEMENT_3D ( 'NONE', #1948, #1314, #2176 ) ;
#10190 = ORIENTED_EDGE ( 'NONE', *, *, #9521, .F. ) ;
#10191 = DIRECTION ( 'NONE',  ( 0.000000000000000000, 0.000000000000000000, 1.000000000000000000 ) ) ;
#10192 = CARTESIAN_POINT ( 'NONE',  ( -8.799590028668788477, 7.703979956833879150, 10.00000000000000000 ) ) ;
#10193 = DIRECTION ( 'NONE',  ( 0.000000000000000000, 0.000000000000000000, -1.000000000000000000 ) ) ;
#10194 = ADVANCED_FACE ( 'NONE', ( #422 ), #10522, .T. ) ;
#10195 = DIRECTION ( 'NONE',  ( 0.000000000000000000, -0.1045284632676605485, 0.9945218953682725127 ) ) ;
#10196 = CIRCLE ( 'NONE', #11954, 24.80000000000000071 ) ;
#10197 = CARTESIAN_POINT ( 'NONE',  ( 2.355103038863950893, 10.93470652055903791, 3.747395293195558847E-16 ) ) ;
#10198 = CIRCLE ( 'NONE', #4928, 9.599999999999997868 ) ;
#10199 = DIRECTION ( 'NONE',  ( -1.000000000000000000, 0.000000000000000000, -0.000000000000000000 ) ) ;
#10200 = EDGE_CURVE ( 'NONE', #8183, #1245, #7079, .T. ) ;
#10201 = CARTESIAN_POINT ( 'NONE',  ( 3.000000000000000888, 0.000000000000000000, 0.000000000000000000 ) ) ;
#10202 = ORIENTED_EDGE ( 'NONE', *, *, #6441, .F. ) ;
#10203 = ORIENTED_EDGE ( 'NONE', *, *, #11661, .F. ) ;
#10204 = AXIS2_PLACEMENT_3D ( 'NONE', #7280, #7405, #11937 ) ;
#10205 = ORIENTED_EDGE ( 'NONE', *, *, #5397, .F. ) ;
#10206 = DIRECTION ( 'NONE',  ( 0.000000000000000000, 0.3090169943749415671, 0.9510565162951555296 ) ) ;
#10207 = AXIS2_PLACEMENT_3D ( 'NONE', #7894, #9613, #1230 ) ;
#10208 = CARTESIAN_POINT ( 'NONE',  ( 0.000000000000000000, 2.811977935938088535, -22.37663021667340857 ) ) ;
#10209 = ADVANCED_FACE ( 'NONE', ( #8879, #2262 ), #5944, .F. ) ;
#10210 = AXIS2_PLACEMENT_3D ( 'NONE', #1142, #1267, #1208 ) ;
#10211 = DIRECTION ( 'NONE',  ( -1.000000000000000000, -0.000000000000000000, -0.000000000000000000 ) ) ;
#10212 = CARTESIAN_POINT ( 'NONE',  ( 1.499999999999999556, 24.75110766671654616, -1.556492618230384872 ) ) ;
#10213 = DIRECTION ( 'NONE',  ( 0.000000000000000000, 0.000000000000000000, -1.000000000000000000 ) ) ;
#10214 = CIRCLE ( 'NONE', #11800, 9.599999999999996092 ) ;
#10215 = CARTESIAN_POINT ( 'NONE',  ( 13.68367311611256554, -8.822018488634762790, 3.747395293195558847E-16 ) ) ;
#10216 = CARTESIAN_POINT ( 'NONE',  ( -0.8869411547437818788, -7.669649013129171244, 6.857782953271941950E-17 ) ) ;
#10217 = CIRCLE ( 'NONE', #2604, 9.599999999999997868 ) ;
#10218 = CARTESIAN_POINT ( 'NONE',  ( 1.499999999999999556, 24.45282072769606430, -4.135161237383341515 ) ) ;
#10219 = ORIENTED_EDGE ( 'NONE', *, *, #5486, .T. ) ;
#10220 = EDGE_LOOP ( 'NONE', ( #9145, #2687, #2032, #3751 ) ) ;
#10221 = VECTOR ( 'NONE', #8110, 1000.000000000000000 ) ;
#10222 = CARTESIAN_POINT ( 'NONE',  ( 0.000000000000000000, 24.75110766671654616, -1.556492618230386649 ) ) ;
#10223 = ORIENTED_EDGE ( 'NONE', *, *, #4340, .F. ) ;
#10224 = EDGE_LOOP ( 'NONE', ( #10937, #11089, #9599, #1561 ) ) ;
#10225 = CARTESIAN_POINT ( 'NONE',  ( 3.006682760306614632, 4.002877712838978752, 10.00000000000000000 ) ) ;
#10226 = DIRECTION ( 'NONE',  ( -1.000000000000000000, 0.000000000000000000, 0.000000000000000000 ) ) ;
#10227 = ORIENTED_EDGE ( 'NONE', *, *, #549, .F. ) ;
#10228 = CARTESIAN_POINT ( 'NONE',  ( 3.000000000000000888, 7.402892494506291499, 21.30300407174365063 ) ) ;
#10229 = DIRECTION ( 'NONE',  ( 0.000000000000000000, 0.000000000000000000, 1.000000000000000000 ) ) ;
#10230 = CARTESIAN_POINT ( 'NONE',  ( -1.032305814202113092, 6.265050879046242471, 10.00000000000000000 ) ) ;
#10231 = SURFACE_STYLE_FILL_AREA ( #7910 ) ;
#10232 = DIRECTION ( 'NONE',  ( -0.000000000000000000, -0.000000000000000000, -1.000000000000000000 ) ) ;
#10233 = CIRCLE ( 'NONE', #4962, 24.80000000000000071 ) ;
#10234 = ORIENTED_EDGE ( 'NONE', *, *, #4639, .T. ) ;
#10235 = EDGE_LOOP ( 'NONE', ( #3309, #2230, #6206, #326 ) ) ;
#10236 = DIRECTION ( 'NONE',  ( 0.000000000000000000, 0.000000000000000000, 1.000000000000000000 ) ) ;
#10237 = ORIENTED_EDGE ( 'NONE', *, *, #523, .F. ) ;
#10238 = CARTESIAN_POINT ( 'NONE',  ( 7.402789038520869447, -0.9464297003978341394, 3.747395293195558847E-16 ) ) ;
#10239 = CARTESIAN_POINT ( 'NONE',  ( 1.500000000000000444, -11.02759168516760013, 22.21333432029560129 ) ) ;
#10240 =( NAMED_UNIT ( * ) PLANE_ANGLE_UNIT ( ) SI_UNIT ( $, .RADIAN. ) );
#10241 = AXIS2_PLACEMENT_3D ( 'NONE', #7231, #8225, #6389 ) ;
#10242 = CARTESIAN_POINT ( 'NONE',  ( 8.000000000000000000, 0.000000000000000000, 19.99999999999999645 ) ) ;
#10243 = EDGE_CURVE ( 'NONE', #3895, #11729, #4098, .T. ) ;
#10244 = DIRECTION ( 'NONE',  ( 0.000000000000000000, 0.000000000000000000, -1.000000000000000000 ) ) ;
#10245 = CARTESIAN_POINT ( 'NONE',  ( -16.00307013876015461, -1.840746716621879830, 10.00000000000000000 ) ) ;
#10247 = EDGE_CURVE ( 'NONE', #9423, #7806, #3786, .T. ) ;
#10246 = CARTESIAN_POINT ( 'NONE',  ( 1.661435237661581521, -7.700870200009177324, 6.857782953271941950E-17 ) ) ;
#10248 = EDGE_CURVE ( 'NONE', #1013, #6911, #11015, .T. ) ;
#10249 = LINE ( 'NONE', #760, #10165 ) ;
#10250 = ORIENTED_EDGE ( 'NONE', *, *, #9886, .F. ) ;
#10251 = ORIENTED_EDGE ( 'NONE', *, *, #846, .F. ) ;
#10252 = AXIS2_PLACEMENT_3D ( 'NONE', #5896, #7037, #2337 ) ;
#10253 = VERTEX_POINT ( 'NONE', #11503 ) ;
#10254 = CARTESIAN_POINT ( 'NONE',  ( 0.000000000000000000, -23.24434456306319419, -8.645255683529242674 ) ) ;
#10255 = CARTESIAN_POINT ( 'NONE',  ( 9.962304844536470583, 3.945508033568877249, 10.00000000000000000 ) ) ;
#10256 = EDGE_CURVE ( 'NONE', #8647, #6529, #5744, .T. ) ;
#10257 = FACE_OUTER_BOUND ( 'NONE', #2530, .T. ) ;
#10258 = CYLINDRICAL_SURFACE ( 'NONE', #4082, 24.80000000000000071 ) ;
#10259 = EDGE_CURVE ( 'NONE', #10253, #6369, #11624, .T. ) ;
#10260 = CARTESIAN_POINT ( 'NONE',  ( -5.868204859621548586, -7.421994279450896848, 3.747395293195558847E-16 ) ) ;
#10261 = CARTESIAN_POINT ( 'NONE',  ( 0.000000000000000000, -23.24434456306331143, 8.645255683528922930 ) ) ;
#10262 = CARTESIAN_POINT ( 'NONE',  ( 0.000000000000000000, 21.97817939804039611, 11.48910920600691554 ) ) ;
#10263 = ORIENTED_EDGE ( 'NONE', *, *, #5767, .T. ) ;
#10264 = VERTEX_POINT ( 'NONE', #10705 ) ;
#10265 = VERTEX_POINT ( 'NONE', #2319 ) ;
#10266 = LINE ( 'NONE', #7508, #11212 ) ;
#10267 = DIRECTION ( 'NONE',  ( 0.000000000000000000, 0.000000000000000000, 1.000000000000000000 ) ) ;
#10268 = SURFACE_STYLE_USAGE ( .BOTH. , #2679 ) ;
#10269 = DIRECTION ( 'NONE',  ( 3.061616997868383141E-16, -1.128098818916242718E-15, 1.000000000000000000 ) ) ;
#10270 = CARTESIAN_POINT ( 'NONE',  ( 0.000000000000000000, 9.589108953448178596, -20.41249101028201451 ) ) ;
#10271 = CARTESIAN_POINT ( 'NONE',  ( 15.52845182490561271, -5.270724383582042094, 3.747395293195558847E-16 ) ) ;
#10272 = CARTESIAN_POINT ( 'NONE',  ( 3.534825977509324257, -7.171832907601985774, 6.857782953271941950E-17 ) ) ;
#10273 = CIRCLE ( 'NONE', #4613, 24.80000000000000071 ) ;
#10274 = DIRECTION ( 'NONE',  ( -1.000000000000000000, 0.000000000000000000, 0.000000000000000000 ) ) ;
#10275 = ORIENTED_EDGE ( 'NONE', *, *, #4216, .F. ) ;
#10276 = ORIENTED_EDGE ( 'NONE', *, *, #11923, .F. ) ;
#10277 = CYLINDRICAL_SURFACE ( 'NONE', #11165, 22.99899999999999878 ) ;
#10278 = VERTEX_POINT ( 'NONE', #9785 ) ;
#10279 = VERTEX_POINT ( 'NONE', #1406 ) ;
#10280 = CARTESIAN_POINT ( 'NONE',  ( 0.000000000000000000, 17.71842311621530186, 17.35216073792446423 ) ) ;
#10281 = EDGE_CURVE ( 'NONE', #9071, #4609, #5546, .T. ) ;
#10282 = DIRECTION ( 'NONE',  ( -1.000000000000000000, 0.000000000000000000, 0.000000000000000000 ) ) ;
#10283 = AXIS2_PLACEMENT_3D ( 'NONE', #4673, #8531, #3872 ) ;
#10284 = ORIENTED_EDGE ( 'NONE', *, *, #2854, .T. ) ;
#10285 = DIRECTION ( 'NONE',  ( 0.000000000000000000, 1.000000000000000000, 3.614007241618348376E-15 ) ) ;
#10286 = CARTESIAN_POINT ( 'NONE',  ( 3.000000000000000888, -2.745295967526151237, 22.83456483164687967 ) ) ;
#10287 = CARTESIAN_POINT ( 'NONE',  ( -4.859750766525547050, 4.557676925202722273, 10.00000000000000000 ) ) ;
#10288 = CARTESIAN_POINT ( 'NONE',  ( 0.000000000000000000, -20.86861857134741172, 9.667200211209745930 ) ) ;
#10289 = EDGE_CURVE ( 'NONE', #962, #6987, #656, .T. ) ;
#10290 = DIRECTION ( 'NONE',  ( -1.000000000000000000, 0.000000000000000000, -0.000000000000000000 ) ) ;
#10291 = ORIENTED_EDGE ( 'NONE', *, *, #10322, .T. ) ;
#10292 = AXIS2_PLACEMENT_3D ( 'NONE', #5136, #1283, #3186 ) ;
#10293 = ORIENTED_EDGE ( 'NONE', *, *, #7322, .F. ) ;
#10294 = CARTESIAN_POINT ( 'NONE',  ( 3.000000000000000888, 0.000000000000000000, 0.000000000000000000 ) ) ;
#10295 = ORIENTED_EDGE ( 'NONE', *, *, #11615, .F. ) ;
#10296 = CARTESIAN_POINT ( 'NONE',  ( 10.01890055165175042, -12.63311126014650121, 10.00000000000000000 ) ) ;
#10297 = DIRECTION ( 'NONE',  ( -1.000000000000000000, 0.000000000000000000, 0.000000000000000000 ) ) ;
#10298 = PRESENTATION_STYLE_ASSIGNMENT (( #188 ) ) ;
#10299 = DIRECTION ( 'NONE',  ( -1.000000000000000000, 0.000000000000000000, 0.000000000000000000 ) ) ;
#10300 = CARTESIAN_POINT ( 'NONE',  ( 3.000000000000000888, 19.29833442572359559, 11.67026512804553562 ) ) ;
#10301 = CARTESIAN_POINT ( 'NONE',  ( -12.80690425020244128, 9.177692349400032867, 10.00000000000000000 ) ) ;
#10302 = CARTESIAN_POINT ( 'NONE',  ( -4.859750766526011567, 4.557676925202717833, 6.857782953271941950E-17 ) ) ;
#10303 = CARTESIAN_POINT ( 'NONE',  ( 3.000000000000000888, 0.000000000000000000, 0.000000000000000000 ) ) ;
#10304 = CYLINDRICAL_SURFACE ( 'NONE', #2743, 19.99999999999999645 ) ;
#10305 = ORIENTED_EDGE ( 'NONE', *, *, #825, .T. ) ;
#10306 = ORIENTED_EDGE ( 'NONE', *, *, #3248, .F. ) ;
#10307 = AXIS2_PLACEMENT_3D ( 'NONE', #6446, #6268, #2473 ) ;
#10308 = CARTESIAN_POINT ( 'NONE',  ( 3.000000000000000888, 24.75110766671654261, -1.556492618230388425 ) ) ;
#10309 = CARTESIAN_POINT ( 'NONE',  ( -0.1586286459269548865, 8.284426055182342097, 10.00000000000000000 ) ) ;
#10310 = B_SPLINE_SURFACE_WITH_KNOTS ( 'NONE', 1, 3, ( 
 ( #9266, #9200, #942, #1796, #3639, #7293, #7355, #10181, #3697, #2780, #4677, #885, #5724, #6566, #3763, #1919, #3580, #8412, #8226, #11229, #6509, #11, #11046, #2657, #8481, #10245, #5594, #7484, #2842, #9448, #6390, #10301, #10114, #5655, #3822, #1008, #4742, #78, #7542, #11287, #2902, #6803, #5897, #11464, #3204, #9628, #2222, #317, #1249, #3138, #6923, #7727, #191, #1300, #8534, #7668, #5959, #10424, #131, #3029, #10539, #2044, #4055, #377, #10667, #7787, #10606, #1069, #5782, #9686, #5035, #6686, #4982, #2967, #6012, #11587, #6863, #11519, #3944, #2158, #8716, #2099, #2278, #8773, #9504, #4116, #1121, #7851, #5838, #4854, #4798, #10483, #8594, #3878, #11406, #6746, #259, #1178, #7599, #9566, #11342, #4920, #8660, #4001, #3085, #9922, #9741, #4356, #5154, #2458, #1359, #4181, #11874, #439, #10967, #558, #9009, #3445, #2399, #498, #1539, #7909, #4417, #5216, #9808, #4292, #11640, #6256, #5276, #5091, #8092, #8024, #11761, #3386, #7098, #5344, #6140, #3258, #9983, #6977, #10722, #3506, #10789, #11820, #1608, #2338, #1422, #10849, #2520, #625, #9869, #8836, #6073, #8893, #7218, #4236, #2590, #6197, #7155, #10903, #1481, #7962, #9074, #11696, #8149, #8947, #3316, #685, #7038, #2830, #1846, #10044, #926, #9253, #872, #8337, #3680, #1905, #2701, #9128, #6553, #11934, #7279, #63, #7339, #4663, #10287, #4474, #6378, #4606, #11215, #10230, #6436, #5400, #5638, #5521, #11086, #7404, #10101, #3809, #7529, #10164, #1665, #5581, #9371, #8210, #11148, #1779 ),
 ( #3567, #739, #989, #4730, #2762, #12058, #11030, #9181, #5452, #2644, #8467, #1718, #803, #11273, #5493, #6494, #9313, #7467, #8397, #4546, #6324, #3744, #8277, #12002, #3624, #9434, #2143, #2027, #9614, #6848, #5821, #1288, #4101, #5705, #7715, #6786, #5883, #305, #8759, #4043, #6610, #10592, #244, #10409, #11327, #11450, #2886, #7767, #3924, #5023, #10344, #4839, #2948, #1963, #11505, #10524, #5946, #7649, #1231, #8641, #11392, #6732, #1053, #1165, #5765, #3013, #359, #8705, #4968, #9490, #3988, #3069, #10466, #7834, #3128, #8521, #2205, #7584, #9673, #2085, #120, #4782, #177, #1107, #3863, #6670, #8578, #9551, #4904, #4279, #3242, #9059, #1525, #10835, #8994, #6910, #11746, #11571, #6185, #6963, #8007, #3191, #6000, #1591, #2266, #671, #2383, #2445, #5259, #4222, #2322, #3370, #9728, #6242, #7023, #11627, #6123, #1344, #8076, #7082, #10653, #9911, #9857, #1467, #5202, #8937, #7143, #7950, #5076, #11805, #8819, #424, #5326, #485, #608, #3435, #4169, #10707, #543, #4342, #10893, #11680, #7895, #2504, #10770, #3299, #9967, #6059, #4401, #9788, #1408, #5141, #8881, #7453, #10028, #857, #8258, #724, #12043, #3727, #1764, #4590, #6418, #10272, #8322, #9297, #7384, #3664, #10216, #1890, #2684, #7261, #8382, #3492, #2629, #914, #5387, #7202, #10086, #5505, #9114, #11127, #11200, #5624, #2747, #5567, #8136, #4460, #4647, #12100, #1653, #6478, #8195, #971, #3550, #10950, #11919, #6363, #7321, #11984, #1831, #11018, #9354, #2816, #6540, #11861, #2570, #6307 ) ),
 .UNSPECIFIED., .F., .F., .F.,
 ( 2, 2 ),
 ( 4, 2, 2, 2, 2, 2, 2, 2, 2, 2, 2, 2, 2, 2, 2, 2, 2, 2, 2, 2, 2, 2, 2, 2, 2, 2, 2, 2, 2, 2, 2, 2, 2, 2, 2, 2, 2, 2, 2, 2, 2, 2, 2, 2, 2, 2, 2, 2, 2, 2, 2, 2, 2, 2, 2, 2, 2, 2, 2, 2, 2, 2, 2, 2, 2, 2, 2, 2, 2, 2, 2, 2, 2, 2, 2, 2, 2, 2, 2, 2, 2, 2, 2, 2, 2, 2, 2, 2, 2, 2, 2, 2, 2, 2, 2, 2, 2, 2, 2, 2, 2, 2, 2, 4 ),
 ( 0.000000000000000000, 0.4545454545454546968 ),
 ( 0.000000000000000000, 0.007812500000000000000, 0.01562500000000000000, 0.02343750000000000000, 0.03125000000000000000, 0.03906250000000000000, 0.04687500000000000000, 0.05468750000000000000, 0.06250000000000000000, 0.07031250000000000000, 0.07812500000000000000, 0.08593750000000000000, 0.09375000000000000000, 0.1015625000000000000, 0.1093750000000000000, 0.1171875000000000000, 0.1250000000000000000, 0.1328125000000000000, 0.1406250000000000000, 0.1484375000000000000, 0.1562500000000000000, 0.1640625000000000000, 0.1718750000000000000, 0.1796875000000000000, 0.1875000000000000000, 0.1953125000000000000, 0.2031250000000000000, 0.2109375000000000000, 0.2187500000000000000, 0.2265625000000000000, 0.2343750000000000000, 0.2421875000000000000, 0.2500000000000000000, 0.2578125000000000000, 0.2656250000000000000, 0.2734375000000000000, 0.2812500000000000000, 0.2890625000000000000, 0.2968750000000000000, 0.3046875000000000000, 0.3125000000000000000, 0.3203125000000000000, 0.3281250000000000000, 0.3359375000000000000, 0.3437500000000000000, 0.3515625000000000000, 0.3593750000000000000, 0.3671875000000000000, 0.3750000000000000000, 0.3828125000000000000, 0.3906250000000000000, 0.3984375000000000000, 0.4062500000000000000, 0.4140625000000000000, 0.4218750000000000000, 0.4296875000000000000, 0.4375000000000000000, 0.4453125000000000000, 0.4531250000000000000, 0.4609375000000000000, 0.4687500000000000000, 0.4765625000000000000, 0.4843750000000000000, 0.4921875000000000000, 0.5000000000000000000, 0.5078125000000000000, 0.5156250000000000000, 0.5234375000000000000, 0.5312500000000000000, 0.5390625000000000000, 0.5468750000000000000, 0.5546875000000000000, 0.5625000000000000000, 0.5703125000000000000, 0.5781250000000000000, 0.5859375000000000000, 0.5937500000000000000, 0.6015625000000000000, 0.6093750000000000000, 0.6171875000000000000, 0.6250000000000000000, 0.6328125000000000000, 0.6406250000000000000, 0.6484375000000000000, 0.6562500000000000000, 0.6640625000000000000, 0.6718750000000000000, 0.6796875000000000000, 0.6875000000000000000, 0.6953125000000000000, 0.7031250000000000000, 0.7109375000000000000, 0.7187500000000000000, 0.7265625000000000000, 0.7343750000000000000, 0.7421875000000000000, 0.7500000000000000000, 0.7656250000000000000, 0.7812500000000000000, 0.7968750000000000000, 0.8125000000000000000, 0.8281250000000000000, 0.8437500000000000000, 0.8499999999999999778 ),
 .UNSPECIFIED. ) ;
#10311 = FACE_OUTER_BOUND ( 'NONE', #2806, .T. ) ;
#10312 = CARTESIAN_POINT ( 'NONE',  ( -8.799590028668786701, 7.703979956834778875, 3.747395293195558847E-16 ) ) ;
#10313 = ADVANCED_FACE ( 'NONE', ( #10947, #2568 ), #8935, .F. ) ;
#10314 = CIRCLE ( 'NONE', #4656, 24.80000000000000071 ) ;
#10315 = LINE ( 'NONE', #8496, #9403 ) ;
#10316 = VERTEX_POINT ( 'NONE', #3433 ) ;
#10317 = PRODUCT_DEFINITION ( 'UNKNOWN', '', #9189, #720 ) ;
#10318 = EDGE_LOOP ( 'NONE', ( #7506, #4005, #3123, #8667 ) ) ;
#10319 = EDGE_CURVE ( 'NONE', #11133, #6834, #3402, .T. ) ;
#10320 = EDGE_LOOP ( 'NONE', ( #6344, #324, #4046, #11841 ) ) ;
#10321 = DIRECTION ( 'NONE',  ( -1.000000000000000000, 0.000000000000000000, 0.000000000000000000 ) ) ;
#10322 = EDGE_CURVE ( 'NONE', #363, #9888, #8081, .T. ) ;
#10323 = CARTESIAN_POINT ( 'NONE',  ( 3.000000000000000888, -4.445336973060693531, -22.56530478845653676 ) ) ;
#10324 = VECTOR ( 'NONE', #5805, 999.9999999999998863 ) ;
#10325 = FACE_OUTER_BOUND ( 'NONE', #5419, .T. ) ;
#10326 = DIRECTION ( 'NONE',  ( 1.000000000000000000, 0.000000000000000000, -0.000000000000000000 ) ) ;
#10327 = CIRCLE ( 'NONE', #4665, 24.80000000000000071 ) ;
#10328 = DIRECTION ( 'NONE',  ( -1.000000000000000000, -0.000000000000000000, -0.000000000000000000 ) ) ;
#10329 = CARTESIAN_POINT ( 'NONE',  ( 1.629745903656676376, 14.14889381255349932, 3.747395293195558847E-16 ) ) ;
#10330 = DIRECTION ( 'NONE',  ( -1.000000000000000000, 0.000000000000000000, 0.000000000000000000 ) ) ;
#10331 = DIRECTION ( 'NONE',  ( 0.000000000000000000, -0.9135454576426046414, 0.4067366430757920481 ) ) ;
#10332 = AXIS2_PLACEMENT_3D ( 'NONE', #11385, #6723, #5815 ) ;
#10333 = VERTEX_POINT ( 'NONE', #5324 ) ;
#10334 = ORIENTED_EDGE ( 'NONE', *, *, #8904, .T. ) ;
#10335 = CARTESIAN_POINT ( 'NONE',  ( 17.24531215409499296, -2.853661713830125013, 10.00000000000000000 ) ) ;
#10336 = EDGE_LOOP ( 'NONE', ( #773, #1522, #11331, #4580 ) ) ;
#10337 = CARTESIAN_POINT ( 'NONE',  ( 1.631735293711821022, 4.895207720155140940, 10.00000000000000000 ) ) ;
#10338 = DIRECTION ( 'NONE',  ( -1.000000000000000000, -0.000000000000000000, -0.000000000000000000 ) ) ;
#10339 = ORIENTED_EDGE ( 'NONE', *, *, #207, .T. ) ;
#10340 = AXIS2_PLACEMENT_3D ( 'NONE', #2376, #9849, #10123 ) ;
#10341 = LINE ( 'NONE', #7527, #9246 ) ;
#10342 = ADVANCED_FACE ( 'NONE', ( #2381 ), #1523, .T. ) ;
#10343 = DIRECTION ( 'NONE',  ( -1.000000000000000000, 0.000000000000000000, -0.000000000000000000 ) ) ;
#10344 = CARTESIAN_POINT ( 'NONE',  ( 14.27634331491212016, 3.322769473268863738, 6.857782953271941950E-17 ) ) ;
#10345 = PLANE ( 'NONE',  #8463 ) ;
#10346 = EDGE_CURVE ( 'NONE', #9959, #5148, #8281, .T. ) ;
#10347 = DIRECTION ( 'NONE',  ( 1.000000000000000000, 0.000000000000000000, 0.000000000000000000 ) ) ;
#10348 = VERTEX_POINT ( 'NONE', #11803 ) ;
#10349 = VERTEX_POINT ( 'NONE', #8133 ) ;
#10350 = CYLINDRICAL_SURFACE ( 'NONE', #9396, 24.80000000000000071 ) ;
#10351 = VERTEX_POINT ( 'NONE', #10833 ) ;
#10352 = CARTESIAN_POINT ( 'NONE',  ( 4.977139221860650942, 13.21892491369670530, 10.00000000000000000 ) ) ;
#10353 = CARTESIAN_POINT ( 'NONE',  ( 0.000000000000000000, 0.000000000000000000, 0.000000000000000000 ) ) ;
#10354 = ADVANCED_FACE ( 'NONE', ( #668 ), #5435, .T. ) ;
#10355 = APPLICATION_CONTEXT ( 'automotive_design' ) ;
#10356 = DIRECTION ( 'NONE',  ( 1.000000000000000000, -0.000000000000000000, -0.000000000000000000 ) ) ;
#10357 = DIRECTION ( 'NONE',  ( 0.000000000000000000, 0.000000000000000000, 1.000000000000000000 ) ) ;
#10358 = CARTESIAN_POINT ( 'NONE',  ( 0.000000000000000000, 21.14796121233196402, 9.039786367038912474 ) ) ;
#10359 = AXIS2_PLACEMENT_3D ( 'NONE', #6629, #11234, #1012 ) ;
#10360 = CARTESIAN_POINT ( 'NONE',  ( 0.000000000000000000, 13.79477846460795831, 18.40266524480593802 ) ) ;
#10361 = LINE ( 'NONE', #4560, #11977 ) ;
#10362 = CIRCLE ( 'NONE', #4888, 24.80000000000000071 ) ;
#10363 = CARTESIAN_POINT ( 'NONE',  ( 3.000000000000000888, 17.97274125076092233, -13.62355943574001671 ) ) ;
#10364 = DIRECTION ( 'NONE',  ( -1.000000000000000000, -0.000000000000000000, 0.000000000000000000 ) ) ;
#10365 = ORIENTED_EDGE ( 'NONE', *, *, #3856, .T. ) ;
#10366 = CARTESIAN_POINT ( 'NONE',  ( -10.00000000000000000, 0.000000000000000000, 0.000000000000000000 ) ) ;
#10367 = VERTEX_POINT ( 'NONE', #4277 ) ;
#10368 = CIRCLE ( 'NONE', #8219, 22.99900000000000233 ) ;
#10369 = CARTESIAN_POINT ( 'NONE',  ( 3.000000000000000888, 0.000000000000000000, 0.000000000000000000 ) ) ;
#10370 = CIRCLE ( 'NONE', #10958, 24.80000000000000071 ) ;
#10371 = CARTESIAN_POINT ( 'NONE',  ( -1.307086582043127443, 11.26718560147321568, 10.00000000000000000 ) ) ;
#10372 = CIRCLE ( 'NONE', #1382, 9.599999999999997868 ) ;
#10373 = CARTESIAN_POINT ( 'NONE',  ( 0.000000000000000000, 24.45282072769601101, 4.135161237383664812 ) ) ;
#10374 = COLOUR_RGB ( '', 0.66274510, 0.83137255, 0.94901961) ;
#10375 = CARTESIAN_POINT ( 'NONE',  ( 10.50580257846853982, 1.391709641844861123, 3.747395293195558847E-16 ) ) ;
#10376 = AXIS2_PLACEMENT_3D ( 'NONE', #10166, #9183, #2704 ) ;
#10377 = CARTESIAN_POINT ( 'NONE',  ( 3.000000000000000888, 6.668524164681944200, -23.88662356770108985 ) ) ;
#10378 = CIRCLE ( 'NONE', #602, 22.99899999999999523 ) ;
#10379 = ORIENTED_EDGE ( 'NONE', *, *, #10888, .T. ) ;
#10380 = CIRCLE ( 'NONE', #4910, 9.599999999999997868 ) ;
#10381 = ORIENTED_EDGE ( 'NONE', *, *, #6912, .T. ) ;
#10382 = EDGE_LOOP ( 'NONE', ( #4941, #1417, #3290, #2999 ) ) ;
#10383 = CARTESIAN_POINT ( 'NONE',  ( 1.499999999999999556, -6.168200451485919444, 24.02068490260611000 ) ) ;
#10384 = CARTESIAN_POINT ( 'NONE',  ( 3.000000000000000000, 2.449293598294706119E-15, -19.99999999999999645 ) ) ;
#10385 = VECTOR ( 'NONE', #8959, 1000.000000000000000 ) ;
#10386 = VERTEX_POINT ( 'NONE', #10082 ) ;
#10387 = CARTESIAN_POINT ( 'NONE',  ( 3.000000000000000888, -7.402892494506437160, 21.30300407174360444 ) ) ;
#10388 = CYLINDRICAL_SURFACE ( 'NONE', #10516, 9.599999999999997868 ) ;
#10389 = ORIENTED_EDGE ( 'NONE', *, *, #8239, .T. ) ;
#10390 = CARTESIAN_POINT ( 'NONE',  ( 0.000000000000000000, 0.000000000000000000, 0.000000000000000000 ) ) ;
#10391 = EDGE_CURVE ( 'NONE', #10167, #10826, #2223, .T. ) ;
#10392 = CARTESIAN_POINT ( 'NONE',  ( -10.19073739998278505, -11.62312336453203443, 3.747395293195558847E-16 ) ) ;
#10393 = EDGE_CURVE ( 'NONE', #7927, #10972, #2813, .T. ) ;
#10394 = EDGE_CURVE ( 'NONE', #532, #3460, #9056, .T. ) ;
#10395 = AXIS2_PLACEMENT_3D ( 'NONE', #7669, #2224, #4983 ) ;
#10396 = CARTESIAN_POINT ( 'NONE',  ( 7.228014483236684722E-17, -0.4999999999999993339, 3.000000000000000000 ) ) ;
#10397 = VERTEX_POINT ( 'NONE', #6305 ) ;
#10398 = AXIS2_PLACEMENT_3D ( 'NONE', #7949, #2204, #7766 ) ;
#10399 = ORIENTED_EDGE ( 'NONE', *, *, #3830, .T. ) ;
#10400 = CARTESIAN_POINT ( 'NONE',  ( 15.92723891616543774, -6.911623607273383207, 10.00000000000000000 ) ) ;
#10401 = ORIENTED_EDGE ( 'NONE', *, *, #5873, .F. ) ;
#10402 = CARTESIAN_POINT ( 'NONE',  ( 3.194803811556594653, -2.743189786380181072, 10.00000000000000000 ) ) ;
#10403 = CARTESIAN_POINT ( 'NONE',  ( 1.500000000000000444, -20.93895013827572171, -13.28910708463150492 ) ) ;
#10404 = ORIENTED_EDGE ( 'NONE', *, *, #11783, .F. ) ;
#10405 = ADVANCED_FACE ( 'NONE', ( #11743 ), #8073, .T. ) ;
#10406 = CARTESIAN_POINT ( 'NONE',  ( 3.000000000000000888, 18.40266524480607657, -13.79477846460777357 ) ) ;
#10407 = AXIS2_PLACEMENT_3D ( 'NONE', #2062, #6203, #6822 ) ;
#10408 = DIRECTION ( 'NONE',  ( 0.000000000000000000, 0.9510565162951521989, 0.3090169943749515036 ) ) ;
#10409 = CARTESIAN_POINT ( 'NONE',  ( 7.525577113297162946, 13.03378399180780534, 6.857782953271941950E-17 ) ) ;
#10410 = FACE_OUTER_BOUND ( 'NONE', #5749, .T. ) ;
#10411 = FACE_OUTER_BOUND ( 'NONE', #2210, .T. ) ;
#10412 = ORIENTED_EDGE ( 'NONE', *, *, #6395, .T. ) ;
#10413 = ORIENTED_EDGE ( 'NONE', *, *, #1938, .T. ) ;
#10414 = CARTESIAN_POINT ( 'NONE',  ( 3.000000000000000888, -2.811977935937933104, 22.37663021667342989 ) ) ;
#10415 = ORIENTED_EDGE ( 'NONE', *, *, #4499, .T. ) ;
#10416 = CIRCLE ( 'NONE', #56, 9.599999999999997868 ) ;
#10417 = EDGE_CURVE ( 'NONE', #8297, #9994, #6708, .T. ) ;
#10418 = CARTESIAN_POINT ( 'NONE',  ( 10.44364468045616157, 9.157203537818526584, 10.00000000000000000 ) ) ;
#10419 = CARTESIAN_POINT ( 'NONE',  ( 3.000000000000000888, 0.000000000000000000, 0.000000000000000000 ) ) ;
#10420 = CARTESIAN_POINT ( 'NONE',  ( 17.49999999999999645, 0.000000000000000000, 6.857782953271941950E-17 ) ) ;
#10421 = ADVANCED_FACE ( 'NONE', ( #9165 ), #6182, .T. ) ;
#10422 = CARTESIAN_POINT ( 'NONE',  ( 3.000000000000000888, 0.3433949777334901476, -22.99643626497956461 ) ) ;
#10423 = CARTESIAN_POINT ( 'NONE',  ( 3.000000000000000888, 0.000000000000000000, 0.000000000000000000 ) ) ;
#10424 = CARTESIAN_POINT ( 'NONE',  ( 11.14370178440676007, -8.845034901279914763, 10.00000000000000000 ) ) ;
#10425 = CIRCLE ( 'NONE', #4370, 9.599999999999997868 ) ;
#10426 = DIRECTION ( 'NONE',  ( 0.000000000000000000, -0.6691306063588494668, -0.7431448254774021267 ) ) ;
#10427 = CARTESIAN_POINT ( 'NONE',  ( -3.562082835880472587, -15.28349083755603388, 3.747395293195558847E-16 ) ) ;
#10428 = CARTESIAN_POINT ( 'NONE',  ( 3.000000000000000000, 0.000000000000000000, 0.000000000000000000 ) ) ;
#10429 = ORIENTED_EDGE ( 'NONE', *, *, #5053, .T. ) ;
#10430 = CARTESIAN_POINT ( 'NONE',  ( 0.000000000000000000, 0.000000000000000000, 0.000000000000000000 ) ) ;
#10431 = EDGE_LOOP ( 'NONE', ( #6683, #4539, #7189, #3275 ) ) ;
#10432 = ORIENTED_EDGE ( 'NONE', *, *, #11513, .T. ) ;
#10433 = CIRCLE ( 'NONE', #863, 9.599999999999996092 ) ;
#10434 = CARTESIAN_POINT ( 'NONE',  ( 0.000000000000000000, 0.000000000000000000, 0.000000000000000000 ) ) ;
#10435 = CARTESIAN_POINT ( 'NONE',  ( 5.657123057053187409, 5.504982807385219168, 10.00000000000000000 ) ) ;
#10436 = EDGE_CURVE ( 'NONE', #8511, #11900, #10425, .T. ) ;
#10437 = LINE ( 'NONE', #11420, #6592 ) ;
#10438 = CARTESIAN_POINT ( 'NONE',  ( 9.246005348854476225, -6.405614325510554430, 10.00000000000000000 ) ) ;
#10439 = CARTESIAN_POINT ( 'NONE',  ( -14.76245309360481706, 5.834016798581969532, 6.857782953271941950E-17 ) ) ;
#10440 = CIRCLE ( 'NONE', #4783, 3.000000000000000000 ) ;
#10441 = CARTESIAN_POINT ( 'NONE',  ( 3.000000000000000888, 17.31945870441147406, 15.13242714128125499 ) ) ;
#10442 = ORIENTED_EDGE ( 'NONE', *, *, #11685, .T. ) ;
#10443 = EDGE_CURVE ( 'NONE', #2754, #3254, #1435, .T. ) ;
#10444 = ORIENTED_EDGE ( 'NONE', *, *, #6624, .T. ) ;
#10445 = DIRECTION ( 'NONE',  ( -1.000000000000000000, 0.000000000000000000, -0.000000000000000000 ) ) ;
#10446 = PLANE ( 'NONE',  #4878 ) ;
#10447 = ORIENTED_EDGE ( 'NONE', *, *, #3771, .F. ) ;
#10448 = CIRCLE ( 'NONE', #11429, 22.99899999999999523 ) ;
#10449 = CARTESIAN_POINT ( 'NONE',  ( 3.000000000000000888, 0.000000000000000000, 0.000000000000000000 ) ) ;
#10450 = LINE ( 'NONE', #2067, #10324 ) ;
#10451 = DIRECTION ( 'NONE',  ( 0.000000000000000000, -0.9945218953682744001, 0.1045284632676436593 ) ) ;
#10452 = CARTESIAN_POINT ( 'NONE',  ( -4.054747718262373901, -11.96785467447665674, 3.747395293195558847E-16 ) ) ;
#10453 = DIRECTION ( 'NONE',  ( 0.000000000000000000, 0.000000000000000000, 1.000000000000000000 ) ) ;
#10454 = ORIENTED_EDGE ( 'NONE', *, *, #303, .F. ) ;
#10455 = ORIENTED_EDGE ( 'NONE', *, *, #8682, .T. ) ;
#10456 = PRODUCT_CONTEXT ( 'NONE', #10355, 'mechanical' ) ;
#10457 = DIRECTION ( 'NONE',  ( -1.000000000000000000, -0.000000000000000000, 0.000000000000000000 ) ) ;
#10458 = VERTEX_POINT ( 'NONE', #5682 ) ;
#10459 = DIRECTION ( 'NONE',  ( 0.000000000000000000, 0.000000000000000000, 1.000000000000000000 ) ) ;
#10460 = CARTESIAN_POINT ( 'NONE',  ( 4.321204520403006732, 2.017656881711013206, 10.00000000000000000 ) ) ;
#10461 = DIRECTION ( 'NONE',  ( 0.000000000000000000, 0.7431448254773910245, 0.6691306063588619013 ) ) ;
#10462 = ORIENTED_EDGE ( 'NONE', *, *, #1670, .T. ) ;
#10463 = EDGE_CURVE ( 'NONE', #3455, #5418, #7089, .T. ) ;
#10464 = CARTESIAN_POINT ( 'NONE',  ( 3.000000000000000000, 0.000000000000000000, -15.00000000000000000 ) ) ;
#10465 = CYLINDRICAL_SURFACE ( 'NONE', #5518, 9.599999999999997868 ) ;
#10466 = CARTESIAN_POINT ( 'NONE',  ( -10.47176928358604364, -8.303818807687074255, 6.857782953271941950E-17 ) ) ;
#10467 = EDGE_CURVE ( 'NONE', #2284, #6367, #9415, .T. ) ;
#10468 = CARTESIAN_POINT ( 'NONE',  ( 0.000000000000000000, 0.000000000000000000, 10.00000000000000000 ) ) ;
#10469 = ORIENTED_EDGE ( 'NONE', *, *, #6642, .F. ) ;
#10470 = CARTESIAN_POINT ( 'NONE',  ( 8.000000000000000000, 0.000000000000000000, 0.000000000000000000 ) ) ;
#10471 = VERTEX_POINT ( 'NONE', #9235 ) ;
#10472 = ORIENTED_EDGE ( 'NONE', *, *, #7854, .F. ) ;
#10473 = DIRECTION ( 'NONE',  ( -0.000000000000000000, -0.000000000000000000, 1.000000000000000000 ) ) ;
#10474 = ORIENTED_EDGE ( 'NONE', *, *, #4409, .T. ) ;
#10475 = EDGE_CURVE ( 'NONE', #1430, #10068, #3794, .T. ) ;
#10476 = CIRCLE ( 'NONE', #5200, 22.99900000000000233 ) ;
#10477 = CARTESIAN_POINT ( 'NONE',  ( 12.15471013770155295, -5.500887282572486825, 10.00000000000000000 ) ) ;
#10478 = EDGE_CURVE ( 'NONE', #9193, #1445, #3006, .T. ) ;
#10479 = CYLINDRICAL_SURFACE ( 'NONE', #502, 9.599999999999997868 ) ;
#10480 = ADVANCED_FACE ( 'NONE', ( #9295 ), #1829, .T. ) ;
#10481 = CYLINDRICAL_SURFACE ( 'NONE', #11674, 22.99899999999999878 ) ;
#10482 = CARTESIAN_POINT ( 'NONE',  ( 3.000000000000000888, 22.90635393027949007, -2.062268319295327057 ) ) ;
#10483 = CARTESIAN_POINT ( 'NONE',  ( 1.597090680284417807, 12.12373805211591460, 10.00000000000000000 ) ) ;
#10484 = CIRCLE ( 'NONE', #5208, 24.80000000000000071 ) ;
#10485 = CARTESIAN_POINT ( 'NONE',  ( 3.000000000000000888, -21.14796121233203152, 9.039786367038763260 ) ) ;
#10486 = CARTESIAN_POINT ( 'NONE',  ( -3.043536693350106681, 14.07442491708025756, 3.747395293195558847E-16 ) ) ;
#10487 = DIRECTION ( 'NONE',  ( -0.000000000000000000, 0.000000000000000000, 1.000000000000000000 ) ) ;
#10488 = EDGE_LOOP ( 'NONE', ( #12080, #1085, #7147, #6659 ) ) ;
#10489 = DIRECTION ( 'NONE',  ( 0.000000000000000000, 0.000000000000000000, -1.000000000000000000 ) ) ;
#10490 = PRODUCT_DEFINITION_SHAPE ( 'NONE', 'NONE',  #5612 ) ;
#10491 = ORIENTED_EDGE ( 'NONE', *, *, #7139, .T. ) ;
#10492 = VERTEX_POINT ( 'NONE', #6476 ) ;
#10493 = CARTESIAN_POINT ( 'NONE',  ( 0.000000000000000000, 22.54798042742718067, -0.4575788569252652871 ) ) ;
#10494 = CARTESIAN_POINT ( 'NONE',  ( -5.846204292276370396, 1.022993486932170404, 10.00000000000000000 ) ) ;
#10495 = DIRECTION ( 'NONE',  ( -1.000000000000000000, 0.000000000000000000, 0.000000000000000000 ) ) ;
#10496 = CARTESIAN_POINT ( 'NONE',  ( 8.539395351299297943, 0.2748098766782894331, 10.00000000000000000 ) ) ;
#10497 = CARTESIAN_POINT ( 'NONE',  ( -3.251399079312188078, 15.05603916236422180, 6.857782953271941950E-17 ) ) ;
#10498 = CARTESIAN_POINT ( 'NONE',  ( 0.000000000000000000, 9.039786367039127413, -21.14796121233187520 ) ) ;
#10499 = EDGE_LOOP ( 'NONE', ( #6045, #3867 ) ) ;
#10500 = ADVANCED_FACE ( 'NONE', ( #11982 ), #6651, .T. ) ;
#10501 = ORIENTED_EDGE ( 'NONE', *, *, #7199, .F. ) ;
#10502 = LINE ( 'NONE', #11484, #1806 ) ;
#10503 = DIRECTION ( 'NONE',  ( -1.000000000000000000, 0.000000000000000000, 0.000000000000000000 ) ) ;
#10504 = CARTESIAN_POINT ( 'NONE',  ( 0.2749788638910972693, -16.81181333738675221, 6.857782953271941950E-17 ) ) ;
#10505 = CARTESIAN_POINT ( 'NONE',  ( 0.000000000000000000, 0.000000000000000000, 0.000000000000000000 ) ) ;
#10506 = CARTESIAN_POINT ( 'NONE',  ( 0.000000000000000000, -2.062268319295407881, -22.90635393027948297 ) ) ;
#10507 = EDGE_CURVE ( 'NONE', #9240, #2984, #10233, .T. ) ;
#10508 = CIRCLE ( 'NONE', #1719, 22.99899999999999878 ) ;
#10509 = CARTESIAN_POINT ( 'NONE',  ( 9.640149279600553456, 4.768118462334743235, 3.747395293195558847E-16 ) ) ;
#10510 = DIRECTION ( 'NONE',  ( -1.000000000000000000, 0.000000000000000000, 0.000000000000000000 ) ) ;
#10511 = ORIENTED_EDGE ( 'NONE', *, *, #7857, .T. ) ;
#10512 = VERTEX_POINT ( 'NONE', #1761 ) ;
#10513 = DIRECTION ( 'NONE',  ( 0.000000000000000000, -1.000000000000000000, 0.000000000000000000 ) ) ;
#10514 = CARTESIAN_POINT ( 'NONE',  ( 3.000000000000000888, -23.05871956130128808, 9.128825345752948905 ) ) ;
#10515 = ORIENTED_EDGE ( 'NONE', *, *, #7057, .F. ) ;
#10516 = AXIS2_PLACEMENT_3D ( 'NONE', #5564, #9294, #4705 ) ;
#10517 = VECTOR ( 'NONE', #3345, 1000.000000000000000 ) ;
#10518 = DIRECTION ( 'NONE',  ( 0.000000000000000000, -0.8090169943749526693, 0.5877852522924660317 ) ) ;
#10519 = DIRECTION ( 'NONE',  ( -0.000000000000000000, -0.000000000000000000, -1.000000000000000000 ) ) ;
#10520 = DIRECTION ( 'NONE',  ( -1.000000000000000000, 0.000000000000000000, 0.000000000000000000 ) ) ;
#10521 = ORIENTED_EDGE ( 'NONE', *, *, #4034, .F. ) ;
#10522 = CYLINDRICAL_SURFACE ( 'NONE', #11209, 9.599999999999997868 ) ;
#10523 = DIRECTION ( 'NONE',  ( -1.000000000000000000, 0.000000000000000000, -0.000000000000000000 ) ) ;
#10524 = CARTESIAN_POINT ( 'NONE',  ( 13.06601448280974509, -5.920767845834311593, 6.857782953271941950E-17 ) ) ;
#10525 = AXIS2_PLACEMENT_3D ( 'NONE', #10818, #3475, #11905 ) ;
#10526 = AXIS2_PLACEMENT_3D ( 'NONE', #10998, #2730, #4571 ) ;
#10527 = CARTESIAN_POINT ( 'NONE',  ( -10.00000000000000000, 0.000000000000000000, 0.000000000000000000 ) ) ;
#10528 = ORIENTED_EDGE ( 'NONE', *, *, #5158, .T. ) ;
#10529 = FACE_OUTER_BOUND ( 'NONE', #6231, .T. ) ;
#10530 = EDGE_LOOP ( 'NONE', ( #787, #10065, #8236, #4513 ) ) ;
#10531 = CARTESIAN_POINT ( 'NONE',  ( 0.000000000000000000, 20.78471918669860941, 8.753070780933226658 ) ) ;
#10532 = ORIENTED_EDGE ( 'NONE', *, *, #7395, .T. ) ;
#10533 = CARTESIAN_POINT ( 'NONE',  ( 9.623054350189521600, -9.012277985855607909, 10.00000000000000000 ) ) ;
#10534 = CIRCLE ( 'NONE', #2925, 9.599999999999997868 ) ;
#10535 = DIRECTION ( 'NONE',  ( 0.000000000000000000, 0.000000000000000000, 1.000000000000000000 ) ) ;
#10536 = FILL_AREA_STYLE ('',( #8768 ) ) ;
#10537 = CARTESIAN_POINT ( 'NONE',  ( 3.000000000000000888, -9.667200211209685534, -20.86861857134744014 ) ) ;
#10538 = CARTESIAN_POINT ( 'NONE',  ( -20.00000000000000000, 2.449293598294706513E-15, 0.000000000000000000 ) ) ;
#10539 = CARTESIAN_POINT ( 'NONE',  ( 7.619603487155713673, -11.82824555707897218, 10.00000000000000000 ) ) ;
#10540 = DIRECTION ( 'NONE',  ( -1.000000000000000000, -0.000000000000000000, -0.000000000000000000 ) ) ;
#10541 = CARTESIAN_POINT ( 'NONE',  ( 3.000000000000000888, 15.13242714128143440, -17.31945870441131419 ) ) ;
#10542 = ADVANCED_FACE ( 'NONE', ( #3610 ), #3661, .T. ) ;
#10543 = VECTOR ( 'NONE', #3362, 1000.000000000000000 ) ;
#10544 = DIRECTION ( 'NONE',  ( -1.000000000000000000, -0.000000000000000000, 0.000000000000000000 ) ) ;
#10545 = ADVANCED_FACE ( 'NONE', ( #7319 ), #855, .T. ) ;
#10546 = DIRECTION ( 'NONE',  ( -1.000000000000000000, -0.000000000000000000, -0.000000000000000000 ) ) ;
#10547 = CIRCLE ( 'NONE', #9958, 9.599999999999996092 ) ;
#10548 = ORIENTED_EDGE ( 'NONE', *, *, #6147, .T. ) ;
#10549 = ORIENTED_EDGE ( 'NONE', *, *, #866, .T. ) ;
#10550 = CARTESIAN_POINT ( 'NONE',  ( -10.00000000000000000, 0.000000000000000000, 0.000000000000000000 ) ) ;
#10551 = CARTESIAN_POINT ( 'NONE',  ( 4.212679447664378074, 6.814025269448781508, 10.00000000000000000 ) ) ;
#10552 = CARTESIAN_POINT ( 'NONE',  ( 0.000000000000000000, -21.30300407174357957, -7.402892494506506438 ) ) ;
#10553 = AXIS2_PLACEMENT_3D ( 'NONE', #5041, #11591, #10610 ) ;
#10554 = CARTESIAN_POINT ( 'NONE',  ( 9.623984404418655103, 6.889883918979096578, 10.00000000000000000 ) ) ;
#10555 = EDGE_CURVE ( 'NONE', #2310, #348, #5941, .T. ) ;
#10556 = CARTESIAN_POINT ( 'NONE',  ( 2.259453438922057522, -13.68937604509904027, 6.857782953271941950E-17 ) ) ;
#10557 = CARTESIAN_POINT ( 'NONE',  ( 0.000000000000000000, -9.667200211209964422, 20.86861857134731579 ) ) ;
#10558 = FACE_OUTER_BOUND ( 'NONE', #10057, .T. ) ;
#10559 = ORIENTED_EDGE ( 'NONE', *, *, #4598, .T. ) ;
#10560 = AXIS2_PLACEMENT_3D ( 'NONE', #10428, #3207, #10487 ) ;
#10561 = AXIS2_PLACEMENT_3D ( 'NONE', #2505, #6245, #12104 ) ;
#10562 = ORIENTED_EDGE ( 'NONE', *, *, #4868, .F. ) ;
#10563 = CYLINDRICAL_SURFACE ( 'NONE', #10210, 22.99899999999999878 ) ;
#10564 = EDGE_CURVE ( 'NONE', #5933, #2253, #9841, .T. ) ;
#10565 =( GEOMETRIC_REPRESENTATION_CONTEXT ( 3 ) GLOBAL_UNCERTAINTY_ASSIGNED_CONTEXT ( ( #9780 ) ) GLOBAL_UNIT_ASSIGNED_CONTEXT ( ( #5031, #314, #1244 ) ) REPRESENTATION_CONTEXT ( 'NONE', 'WORKASPACE' ) );
#10566 = CARTESIAN_POINT ( 'NONE',  ( 11.04976219204224996, -11.79656285005915350, 10.00000000000000000 ) ) ;
#10567 = EDGE_LOOP ( 'NONE', ( #10990, #8392 ) ) ;
#10568 = CARTESIAN_POINT ( 'NONE',  ( -10.00000000000000000, 0.000000000000000000, 0.000000000000000000 ) ) ;
#10569 = DIRECTION ( 'NONE',  ( 0.000000000000000000, 0.000000000000000000, -1.000000000000000000 ) ) ;
#10570 = CIRCLE ( 'NONE', #3340, 9.599999999999997868 ) ;
#10571 = EDGE_CURVE ( 'NONE', #3166, #4944, #1250, .T. ) ;
#10572 = VECTOR ( 'NONE', #5311, 1000.000000000000000 ) ;
#10573 = VECTOR ( 'NONE', #9794, 1000.000000000000000 ) ;
#10574 = CARTESIAN_POINT ( 'NONE',  ( -10.00031051369627022, 6.213292778946845729, 3.747395293195558847E-16 ) ) ;
#10575 = EDGE_CURVE ( 'NONE', #10781, #1468, #4350, .T. ) ;
#10576 = CARTESIAN_POINT ( 'NONE',  ( 3.500000000000000000, 0.000000000000000000, -15.00000000000000000 ) ) ;
#10577 = ORIENTED_EDGE ( 'NONE', *, *, #5481, .F. ) ;
#10578 = VERTEX_POINT ( 'NONE', #11312 ) ;
#10579 = SHAPE_DEFINITION_REPRESENTATION ( #7750, #6315 ) ;
#10580 = CARTESIAN_POINT ( 'NONE',  ( 0.5005346673319861495, 15.27733729710888255, 10.00000000000000000 ) ) ;
#10581 = EDGE_CURVE ( 'NONE', #3718, #7675, #10035, .T. ) ;
#10582 = CIRCLE ( 'NONE', #7846, 9.599999999999999645 ) ;
#10583 = ORIENTED_EDGE ( 'NONE', *, *, #11138, .T. ) ;
#10584 = CARTESIAN_POINT ( 'NONE',  ( 0.000000000000000000, -17.35216073792428304, -17.71842311621547950 ) ) ;
#10585 = DIRECTION ( 'NONE',  ( 0.000000000000000000, 0.000000000000000000, 1.000000000000000000 ) ) ;
#10586 = VECTOR ( 'NONE', #1263, 1000.000000000000000 ) ;
#10587 = CIRCLE ( 'NONE', #807, 24.80000000000000071 ) ;
#10588 = LINE ( 'NONE', #2379, #3646 ) ;
#10589 = ORIENTED_EDGE ( 'NONE', *, *, #11003, .F. ) ;
#10590 = DIRECTION ( 'NONE',  ( 0.000000000000000000, -1.000000000000000000, -1.047444401652940007E-14 ) ) ;
#10591 = DIRECTION ( 'NONE',  ( -1.000000000000000000, -0.000000000000000000, -0.000000000000000000 ) ) ;
#10592 = CARTESIAN_POINT ( 'NONE',  ( 4.165359127293307040, 14.58480927028732843, 6.857782953271941950E-17 ) ) ;
#10593 = VECTOR ( 'NONE', #627, 1000.000000000000000 ) ;
#10594 = VERTEX_POINT ( 'NONE', #3724 ) ;
#10595 = VECTOR ( 'NONE', #6186, 1000.000000000000000 ) ;
#10596 = CARTESIAN_POINT ( 'NONE',  ( 3.000000000000000888, -21.76479567747236743, -7.432877647175426539 ) ) ;
#10597 = CARTESIAN_POINT ( 'NONE',  ( 3.000000000000000888, 4.445336973061170482, -22.56530478845644794 ) ) ;
#10598 = EDGE_CURVE ( 'NONE', #5600, #7059, #7451, .T. ) ;
#10599 = ORIENTED_EDGE ( 'NONE', *, *, #3161, .F. ) ;
#10600 = CARTESIAN_POINT ( 'NONE',  ( 2.355103038863951781, 10.93470652055904146, 10.00000000000000000 ) ) ;
#10601 = CIRCLE ( 'NONE', #631, 9.599999999999996092 ) ;
#10602 = VECTOR ( 'NONE', #4662, 1000.000000000000000 ) ;
#10603 = DIRECTION ( 'NONE',  ( -1.000000000000000000, -0.000000000000000000, -0.000000000000000000 ) ) ;
#10604 = CARTESIAN_POINT ( 'NONE',  ( 0.000000000000000000, 6.668524164681944200, -23.88662356770108630 ) ) ;
#10605 = CARTESIAN_POINT ( 'NONE',  ( 0.000000000000000000, 0.000000000000000000, -15.00000000000000000 ) ) ;
#10606 = CARTESIAN_POINT ( 'NONE',  ( -2.240087900411203758, -13.53314956822678639, 10.00000000000000000 ) ) ;
#10607 = DIRECTION ( 'NONE',  ( 1.000000000000000000, 0.000000000000000000, -0.000000000000000000 ) ) ;
#10608 = CARTESIAN_POINT ( 'NONE',  ( 0.000000000000000000, -20.65684170206481696, -13.72351598154918406 ) ) ;
#10609 = AXIS2_PLACEMENT_3D ( 'NONE', #7500, #92, #9284 ) ;
#10610 = DIRECTION ( 'NONE',  ( 0.000000000000000000, 0.000000000000000000, 1.000000000000000000 ) ) ;
#10611 = ORIENTED_EDGE ( 'NONE', *, *, #6258, .F. ) ;
#10612 = CIRCLE ( 'NONE', #9251, 9.599999999999997868 ) ;
#10613 = EDGE_LOOP ( 'NONE', ( #7521, #9241, #9590, #9674 ) ) ;
#10614 = ORIENTED_EDGE ( 'NONE', *, *, #12045, .T. ) ;
#10615 = CARTESIAN_POINT ( 'NONE',  ( 16.50000000000000000, 0.000000000000000000, 3.747395293195558847E-16 ) ) ;
#10616 = CARTESIAN_POINT ( 'NONE',  ( 7.261170810407329590, -1.543028577657542311, 10.00000000000000000 ) ) ;
#10617 = AXIS2_PLACEMENT_3D ( 'NONE', #9670, #241, #3239 ) ;
#10618 = DIRECTION ( 'NONE',  ( -1.000000000000000000, -0.000000000000000000, -0.000000000000000000 ) ) ;
#10619 = EDGE_CURVE ( 'NONE', #2975, #7896, #6336, .T. ) ;
#10620 = DIRECTION ( 'NONE',  ( -1.000000000000000000, 0.000000000000000000, 0.000000000000000000 ) ) ;
#10621 = CARTESIAN_POINT ( 'NONE',  ( 11.40744677810891083, -1.317628706759891966, 10.00000000000000000 ) ) ;
#10622 = CIRCLE ( 'NONE', #11976, 22.99899999999999878 ) ;
#10623 = AXIS2_PLACEMENT_3D ( 'NONE', #1899, #2018, #55 ) ;
#10624 = CARTESIAN_POINT ( 'NONE',  ( -12.80690425020131684, 9.177692349400029315, 6.857782953271941950E-17 ) ) ;
#10625 = DIRECTION ( 'NONE',  ( 0.000000000000000000, 0.5877852522924690293, 0.8090169943749505599 ) ) ;
#10626 = DIRECTION ( 'NONE',  ( 0.000000000000000000, -0.4067366430758070917, 0.9135454576425978690 ) ) ;
#10627 = ORIENTED_EDGE ( 'NONE', *, *, #8507, .F. ) ;
#10628 = ORIENTED_EDGE ( 'NONE', *, *, #5798, .F. ) ;
#10629 = AXIS2_PLACEMENT_3D ( 'NONE', #7381, #11125, #104 ) ;
#10630 = ORIENTED_EDGE ( 'NONE', *, *, #11892, .T. ) ;
#10631 = ADVANCED_FACE ( 'NONE', ( #7514 ), #11257, .F. ) ;
#10632 = DIRECTION ( 'NONE',  ( 0.000000000000000000, 0.6691306063588543518, 0.7431448254773976858 ) ) ;
#10633 = CARTESIAN_POINT ( 'NONE',  ( 4.123629756450001516, -15.38522696314584870, 10.00000000000000000 ) ) ;
#10634 = ADVANCED_FACE ( 'NONE', ( #11652 ), #7919, .T. ) ;
#10635 = DIRECTION ( 'NONE',  ( -1.000000000000000000, 0.000000000000000000, -0.000000000000000000 ) ) ;
#10636 = DIRECTION ( 'NONE',  ( 1.000000000000000000, 0.000000000000000000, -0.000000000000000000 ) ) ;
#10637 = CIRCLE ( 'NONE', #4776, 9.599999999999997868 ) ;
#10638 = CARTESIAN_POINT ( 'NONE',  ( -9.037587479195730467, -0.7561632655184011842, 3.747395293195558847E-16 ) ) ;
#10639 = CARTESIAN_POINT ( 'NONE',  ( 3.000000000000000888, -22.99643626497957172, 0.3433949777330864706 ) ) ;
#10640 = VERTEX_POINT ( 'NONE', #3404 ) ;
#10641 = ORIENTED_EDGE ( 'NONE', *, *, #8582, .F. ) ;
#10642 =( NAMED_UNIT ( * ) PLANE_ANGLE_UNIT ( ) SI_UNIT ( $, .RADIAN. ) );
#10643 = CARTESIAN_POINT ( 'NONE',  ( 14.22875512193219372, -2.589574901423981501, 10.00000000000000000 ) ) ;
#10644 = EDGE_LOOP ( 'NONE', ( #4843, #9555, #9704, #11396 ) ) ;
#10645 = AXIS2_PLACEMENT_3D ( 'NONE', #11029, #7097, #7338 ) ;
#10646 = DIRECTION ( 'NONE',  ( -1.000000000000000000, 0.000000000000000000, 0.000000000000000000 ) ) ;
#10647 = CYLINDRICAL_SURFACE ( 'NONE', #1242, 9.599999999999997868 ) ;
#10648 = UNCERTAINTY_MEASURE_WITH_UNIT (LENGTH_MEASURE( 1.000000000000000082E-05 ), #1065, 'distance_accuracy_value', 'NONE');
#10649 = DIRECTION ( 'NONE',  ( -0.000000000000000000, -0.000000000000000000, -1.000000000000000000 ) ) ;
#10650 = ORIENTED_EDGE ( 'NONE', *, *, #2406, .F. ) ;
#10651 = DIRECTION ( 'NONE',  ( -1.000000000000000000, -0.000000000000000000, 0.000000000000000000 ) ) ;
#10652 = DIRECTION ( 'NONE',  ( -1.000000000000000000, 0.000000000000000000, 0.000000000000000000 ) ) ;
#10653 = CARTESIAN_POINT ( 'NONE',  ( -5.125696908148159814, -9.212757455309411370, 6.857782953271941950E-17 ) ) ;
#10654 = VERTEX_POINT ( 'NONE', #9881 ) ;
#10655 = DIRECTION ( 'NONE',  ( -1.000000000000000000, 0.000000000000000000, -0.000000000000000000 ) ) ;
#10656 = VERTEX_POINT ( 'NONE', #3215 ) ;
#10657 = CARTESIAN_POINT ( 'NONE',  ( -10.00000000000000000, 0.000000000000000000, 0.000000000000000000 ) ) ;
#10658 = EDGE_LOOP ( 'NONE', ( #1019, #8488, #667, #947 ) ) ;
#10659 = EDGE_CURVE ( 'NONE', #5010, #2665, #6932, .T. ) ;
#10660 = CARTESIAN_POINT ( 'NONE',  ( -5.868204859621552139, -7.421994279450156107, 10.00000000000000000 ) ) ;
#10661 = DIRECTION ( 'NONE',  ( 0.000000000000000000, 0.6691306063588544628, 0.7431448254773976858 ) ) ;
#10662 = AXIS2_PLACEMENT_3D ( 'NONE', #7288, #5355, #6265 ) ;
#10663 = FILL_AREA_STYLE ('',( #9682 ) ) ;
#10664 = DIRECTION ( 'NONE',  ( 1.000000000000000000, 0.000000000000000000, 0.000000000000000000 ) ) ;
#10665 = EDGE_CURVE ( 'NONE', #3976, #4079, #11417, .T. ) ;
#10666 = DIRECTION ( 'NONE',  ( 0.000000000000000000, 0.000000000000000000, 1.000000000000000000 ) ) ;
#10667 = CARTESIAN_POINT ( 'NONE',  ( 1.124919223378051392, -13.78906249641292270, 10.00000000000000000 ) ) ;
#10668 = CARTESIAN_POINT ( 'NONE',  ( 3.000000000000000888, 20.86861857134747922, -9.667200211209612704 ) ) ;
#10669 = CARTESIAN_POINT ( 'NONE',  ( 16.46093749971205611, -1.349437486485979498, 3.747395293195558847E-16 ) ) ;
#10670 = CARTESIAN_POINT ( 'NONE',  ( 0.000000000000000000, 15.40502424595170972, -19.43515443678387555 ) ) ;
#10671 = CIRCLE ( 'NONE', #8915, 9.599999999999997868 ) ;
#10672 = ORIENTED_EDGE ( 'NONE', *, *, #1791, .T. ) ;
#10673 = FACE_OUTER_BOUND ( 'NONE', #4626, .T. ) ;
#10674 = ORIENTED_EDGE ( 'NONE', *, *, #9546, .F. ) ;
#10675 = CARTESIAN_POINT ( 'NONE',  ( 3.000000000000000888, 0.000000000000000000, 0.000000000000000000 ) ) ;
#10676 = CARTESIAN_POINT ( 'NONE',  ( 8.000000000000000000, 2.449293598294706119E-15, -19.99999999999999645 ) ) ;
#10677 = VECTOR ( 'NONE', #11622, 1000.000000000000000 ) ;
#10678 = CARTESIAN_POINT ( 'NONE',  ( 3.000000000000000888, -15.13242714128131361, 17.31945870441142077 ) ) ;
#10679 = CARTESIAN_POINT ( 'NONE',  ( 7.737545192982512532, 9.111483571581279861, 10.00000000000000000 ) ) ;
#10680 = CARTESIAN_POINT ( 'NONE',  ( -9.386162357322611172, -4.067606288967436257, 6.857782953271941950E-17 ) ) ;
#10681 = CARTESIAN_POINT ( 'NONE',  ( 3.000000000000000888, -17.31945870441136748, -15.13242714128137401 ) ) ;
#10682 = FACE_OUTER_BOUND ( 'NONE', #1852, .T. ) ;
#10683 = ORIENTED_EDGE ( 'NONE', *, *, #1124, .F. ) ;
#10684 = VERTEX_POINT ( 'NONE', #3268 ) ;
#10685 = CIRCLE ( 'NONE', #8545, 20.00000000000000000 ) ;
#10686 = VERTEX_POINT ( 'NONE', #5227 ) ;
#10687 = CARTESIAN_POINT ( 'NONE',  ( 0.000000000000000000, 0.000000000000000000, 0.000000000000000000 ) ) ;
#10688 = EDGE_CURVE ( 'NONE', #10512, #843, #8093, .T. ) ;
#10689 = LINE ( 'NONE', #2187, #2311 ) ;
#10690 = CARTESIAN_POINT ( 'NONE',  ( 4.071483724746831179, 10.33449570568845033, 3.747395293195558847E-16 ) ) ;
#10691 = PRODUCT_DEFINITION ( 'UNKNOWN', '', #10756, #4521 ) ;
#10692 = EDGE_CURVE ( 'NONE', #10684, #8706, #665, .T. ) ;
#10693 = DIRECTION ( 'NONE',  ( 1.000000000000000000, 0.000000000000000000, 0.000000000000000000 ) ) ;
#10694 = EDGE_LOOP ( 'NONE', ( #181, #7981, #579, #6954 ) ) ;
#10695 = ORIENTED_EDGE ( 'NONE', *, *, #3454, .F. ) ;
#10696 =( NAMED_UNIT ( * ) SI_UNIT ( $, .STERADIAN. ) SOLID_ANGLE_UNIT ( ) );
#10697 = CARTESIAN_POINT ( 'NONE',  ( -4.389456771235332511, 11.66511648340389762, 10.00000000000000000 ) ) ;
#10698 = EDGE_CURVE ( 'NONE', #8629, #6518, #6715, .T. ) ;
#10699 = VERTEX_POINT ( 'NONE', #4824 ) ;
#10700 = LINE ( 'NONE', #7707, #7978 ) ;
#10701 = DIRECTION ( 'NONE',  ( 0.000000000000000000, -0.5877852522924630341, -0.8090169943749546677 ) ) ;
#10702 = CIRCLE ( 'NONE', #339, 22.00000000000000000 ) ;
#10703 = LINE ( 'NONE', #7015, #4627 ) ;
#10704 = EDGE_LOOP ( 'NONE', ( #10882, #6098, #3571, #4218 ) ) ;
#10705 = CARTESIAN_POINT ( 'NONE',  ( 20.00000000000000000, 0.000000000000000000, 0.000000000000000000 ) ) ;
#10706 = CARTESIAN_POINT ( 'NONE',  ( 3.000000000000000888, 0.000000000000000000, 0.000000000000000000 ) ) ;
#10707 = CARTESIAN_POINT ( 'NONE',  ( -4.625218816436122538, 8.325684435358754243, 6.857782953271941950E-17 ) ) ;
#10708 = ORIENTED_EDGE ( 'NONE', *, *, #11742, .F. ) ;
#10709 = DIRECTION ( 'NONE',  ( -1.000000000000000000, -0.000000000000000000, -0.000000000000000000 ) ) ;
#10710 = CIRCLE ( 'NONE', #1131, 22.99899999999999878 ) ;
#10711 = ORIENTED_EDGE ( 'NONE', *, *, #7857, .F. ) ;
#10712 = CARTESIAN_POINT ( 'NONE',  ( 1.500000000000000444, 11.48910920600683561, 21.97817939804043874 ) ) ;
#10713 = VERTEX_POINT ( 'NONE', #10678 ) ;
#10714 = CARTESIAN_POINT ( 'NONE',  ( 6.391761267591818729, 8.940137919804724831, 10.00000000000000000 ) ) ;
#10715 = EDGE_CURVE ( 'NONE', #5315, #5509, #3803, .T. ) ;
#10716 = CARTESIAN_POINT ( 'NONE',  ( 3.000000000000000888, -22.90635393027947941, 2.062268319295487817 ) ) ;
#10717 = PRESENTATION_STYLE_ASSIGNMENT (( #6973 ) ) ;
#10718 = EDGE_LOOP ( 'NONE', ( #10015, #5573 ) ) ;
#10719 = LINE ( 'NONE', #3136, #2302 ) ;
#10720 = COLOUR_RGB ( '', 0.08235294, 0.09019608, 0.10196078) ;
#10721 = DIRECTION ( 'NONE',  ( 0.000000000000000000, 0.000000000000000000, 1.000000000000000000 ) ) ;
#10722 = CARTESIAN_POINT ( 'NONE',  ( -1.672018190274039418, 9.216430685901391584, 10.00000000000000000 ) ) ;
#10723 = ADVANCED_FACE ( 'NONE', ( #8960 ), #4307, .T. ) ;
#10724 = LINE ( 'NONE', #8894, #10593 ) ;
#10725 = CARTESIAN_POINT ( 'NONE',  ( -7.594692469639082510, -9.901549393537251831, 3.747395293195558847E-16 ) ) ;
#10726 = DIRECTION ( 'NONE',  ( -1.000000000000000000, -0.000000000000000000, -0.000000000000000000 ) ) ;
#10727 = ORIENTED_EDGE ( 'NONE', *, *, #9185, .T. ) ;
#10728 = FACE_OUTER_BOUND ( 'NONE', #11426, .T. ) ;
#10729 = VERTEX_POINT ( 'NONE', #6990 ) ;
#10730 = AXIS2_PLACEMENT_3D ( 'NONE', #3184, #6955, #5014 ) ;
#10731 = ADVANCED_FACE ( 'NONE', ( #6090 ), #5169, .T. ) ;
#10732 = CYLINDRICAL_SURFACE ( 'NONE', #10662, 9.599999999999997868 ) ;
#10733 = ORIENTED_EDGE ( 'NONE', *, *, #1429, .F. ) ;
#10734 = DIRECTION ( 'NONE',  ( -1.000000000000000000, 0.000000000000000000, 0.000000000000000000 ) ) ;
#10735 = DIRECTION ( 'NONE',  ( -1.000000000000000000, -0.000000000000000000, 0.000000000000000000 ) ) ;
#10736 = CARTESIAN_POINT ( 'NONE',  ( -5.248573321596930796, 4.168074790661433049, 10.00000000000000000 ) ) ;
#10737 = AXIS2_PLACEMENT_3D ( 'NONE', #2625, #6358, #10080 ) ;
#10738 = AXIS2_PLACEMENT_3D ( 'NONE', #2496, #7074, #7943 ) ;
#10739 = CARTESIAN_POINT ( 'NONE',  ( -9.960937504979705537, 0.8181230654449899165, 6.857782953271941950E-17 ) ) ;
#10740 = DIRECTION ( 'NONE',  ( -1.000000000000000000, -0.000000000000000000, -0.000000000000000000 ) ) ;
#10741 = CIRCLE ( 'NONE', #2928, 9.599999999999996092 ) ;
#10742 = CARTESIAN_POINT ( 'NONE',  ( 3.000000000000000888, 0.000000000000000000, 0.000000000000000000 ) ) ;
#10743 = ORIENTED_EDGE ( 'NONE', *, *, #9585, .T. ) ;
#10744 = VERTEX_POINT ( 'NONE', #5105 ) ;
#10745 = AXIS2_PLACEMENT_3D ( 'NONE', #4766, #8557, #2926 ) ;
#10746 = CARTESIAN_POINT ( 'NONE',  ( 0.000000000000000000, 2.062268319295562424, 22.90635393027947231 ) ) ;
#10747 = DIRECTION ( 'NONE',  ( 0.000000000000000000, 0.000000000000000000, 1.000000000000000000 ) ) ;
#10748 = CARTESIAN_POINT ( 'NONE',  ( 3.000000000000000888, -14.74749645579999857, -17.06259499759959297 ) ) ;
#10749 = CARTESIAN_POINT ( 'NONE',  ( -5.359287035703753865, 6.724520318540387009, 3.747395293195558847E-16 ) ) ;
#10750 = AXIS2_PLACEMENT_3D ( 'NONE', #5785, #4803, #11411 ) ;
#10751 = DIRECTION ( 'NONE',  ( -1.000000000000000000, -0.000000000000000000, -0.000000000000000000 ) ) ;
#10752 = VECTOR ( 'NONE', #6854, 1000.000000000000000 ) ;
#10753 = CARTESIAN_POINT ( 'NONE',  ( 3.000000000000000888, -6.779701584702581663, -21.97702544527764701 ) ) ;
#10754 = EDGE_LOOP ( 'NONE', ( #616, #1837, #4763, #3806 ) ) ;
#10755 = ORIENTED_EDGE ( 'NONE', *, *, #4345, .F. ) ;
#10756 = PRODUCT_DEFINITION_FORMATION_WITH_SPECIFIED_SOURCE ( 'ANY', '', #8642, .NOT_KNOWN. ) ;
#10757 = CARTESIAN_POINT ( 'NONE',  ( -1.410059164928063380, 12.26527237696110184, 10.00000000000000000 ) ) ;
#10758 = ORIENTED_EDGE ( 'NONE', *, *, #3689, .F. ) ;
#10759 = DIRECTION ( 'NONE',  ( 0.000000000000000000, 0.000000000000000000, 1.000000000000000000 ) ) ;
#10760 = DIRECTION ( 'NONE',  ( -1.000000000000000000, 0.000000000000000000, 0.000000000000000000 ) ) ;
#10761 = DIRECTION ( 'NONE',  ( -1.000000000000000000, -0.000000000000000000, 0.000000000000000000 ) ) ;
#10762 = EDGE_LOOP ( 'NONE', ( #1379, #10641, #8957, #5444 ) ) ;
#10763 = EDGE_CURVE ( 'NONE', #9620, #11676, #11709, .T. ) ;
#10764 = CIRCLE ( 'NONE', #3737, 9.599999999999997868 ) ;
#10765 = AXIS2_PLACEMENT_3D ( 'NONE', #7509, #5618, #42 ) ;
#10766 = DIRECTION ( 'NONE',  ( 0.000000000000000000, 0.000000000000000000, 1.000000000000000000 ) ) ;
#10767 = EDGE_CURVE ( 'NONE', #5179, #6658, #268, .T. ) ;
#10768 = EDGE_CURVE ( 'NONE', #7721, #9363, #8286, .T. ) ;
#10769 = CARTESIAN_POINT ( 'NONE',  ( 3.000000000000000888, -22.56530478845645860, -4.445336973061090546 ) ) ;
#10770 = CARTESIAN_POINT ( 'NONE',  ( 2.798030692818294085, 8.692477993603722197, 6.857782953271941950E-17 ) ) ;
#10771 = ORIENTED_EDGE ( 'NONE', *, *, #596, .F. ) ;
#10772 = DIRECTION ( 'NONE',  ( 0.000000000000000000, -0.2079116908177466583, -0.9781476007338082423 ) ) ;
#10773 = CIRCLE ( 'NONE', #3734, 24.80000000000000071 ) ;
#10774 = ORIENTED_EDGE ( 'NONE', *, *, #10785, .T. ) ;
#10775 = LINE ( 'NONE', #3304, #11938 ) ;
#10776 = CIRCLE ( 'NONE', #5895, 9.599999999999996092 ) ;
#10777 = ORIENTED_EDGE ( 'NONE', *, *, #9833, .F. ) ;
#10778 = VECTOR ( 'NONE', #1517, 1000.000000000000000 ) ;
#10779 = CARTESIAN_POINT ( 'NONE',  ( 10.39479819782869896, 2.258419626871297492, 10.00000000000000000 ) ) ;
#10780 = EDGE_CURVE ( 'NONE', #5379, #8825, #9534, .T. ) ;
#10781 = VERTEX_POINT ( 'NONE', #8623 ) ;
#10782 = CARTESIAN_POINT ( 'NONE',  ( 3.000000000000000888, 22.90635393027946165, 2.062268319295641472 ) ) ;
#10783 = CARTESIAN_POINT ( 'NONE',  ( 5.000000000000000000, 6.123233995736766282E-16, 1.000000000000000000 ) ) ;
#10784 = ORIENTED_EDGE ( 'NONE', *, *, #2571, .F. ) ;
#10785 = EDGE_CURVE ( 'NONE', #6248, #2893, #224, .T. ) ;
#10786 = AXIS2_PLACEMENT_3D ( 'NONE', #6496, #1850, #931 ) ;
#10787 = DIRECTION ( 'NONE',  ( 0.000000000000000000, 0.000000000000000000, 1.000000000000000000 ) ) ;
#10788 = CYLINDRICAL_SURFACE ( 'NONE', #7511, 24.80000000000000071 ) ;
#10789 = CARTESIAN_POINT ( 'NONE',  ( 0.6097887191948987429, 9.229167205757272896, 10.00000000000000000 ) ) ;
#10790 = DIRECTION ( 'NONE',  ( 0.000000000000000000, -0.5000000000000072164, 0.8660254037844344888 ) ) ;
#10791 = CARTESIAN_POINT ( 'NONE',  ( -9.680665087125342794, -7.686621967951971612, 3.747395293195558847E-16 ) ) ;
#10792 = DIRECTION ( 'NONE',  ( -1.000000000000000000, -0.000000000000000000, 0.000000000000000000 ) ) ;
#10793 = EDGE_CURVE ( 'NONE', #8912, #2073, #10433, .T. ) ;
#10794 = VERTEX_POINT ( 'NONE', #4193 ) ;
#10795 = CARTESIAN_POINT ( 'NONE',  ( 1.500000000000000444, 20.93895013827581408, 13.28910708463135215 ) ) ;
#10796 = AXIS2_PLACEMENT_3D ( 'NONE', #5346, #3205, #6015 ) ;
#10797 = VERTEX_POINT ( 'NONE', #3464 ) ;
#10798 = AXIS2_PLACEMENT_3D ( 'NONE', #6552, #3808, #2084 ) ;
#10799 = DIRECTION ( 'NONE',  ( -1.000000000000000000, 0.000000000000000000, 3.061616997868383141E-16 ) ) ;
#10800 = ORIENTED_EDGE ( 'NONE', *, *, #7005, .F. ) ;
#10801 = CARTESIAN_POINT ( 'NONE',  ( 3.000000000000000888, 0.000000000000000000, 0.000000000000000000 ) ) ;
#10802 = CARTESIAN_POINT ( 'NONE',  ( 0.000000000000000000, -17.97274125076083351, 13.62355943574013750 ) ) ;
#10803 = DIRECTION ( 'NONE',  ( -1.000000000000000000, 0.000000000000000000, -0.000000000000000000 ) ) ;
#10804 = CARTESIAN_POINT ( 'NONE',  ( -7.040021908109685533, -0.4595208068205508534, 10.00000000000000000 ) ) ;
#10805 = CIRCLE ( 'NONE', #1416, 9.599999999999996092 ) ;
#10806 = CARTESIAN_POINT ( 'NONE',  ( -11.39998097177137026, 5.856612080558655897, 6.857782953271941950E-17 ) ) ;
#10807 = FILL_AREA_STYLE ('',( #7054 ) ) ;
#10808 = CARTESIAN_POINT ( 'NONE',  ( -5.000000000000000000, 0.000000000000000000, 1.000000000000000000 ) ) ;
#10809 = VERTEX_POINT ( 'NONE', #9088 ) ;
#10810 = ORIENTED_EDGE ( 'NONE', *, *, #12105, .T. ) ;
#10811 = ORIENTED_EDGE ( 'NONE', *, *, #6728, .T. ) ;
#10812 = EDGE_CURVE ( 'NONE', #1739, #6675, #7695, .T. ) ;
#10813 = AXIS2_PLACEMENT_3D ( 'NONE', #2828, #8518, #3921 ) ;
#10814 = CARTESIAN_POINT ( 'NONE',  ( -14.61026919807147451, 3.159152207411757285, 10.00000000000000000 ) ) ;
#10815 = AXIS2_PLACEMENT_3D ( 'NONE', #2924, #8314, #3656 ) ;
#10816 = CYLINDRICAL_SURFACE ( 'NONE', #3682, 24.80000000000000071 ) ;
#10817 = CIRCLE ( 'NONE', #5542, 22.99899999999999523 ) ;
#10818 = CARTESIAN_POINT ( 'NONE',  ( 8.000000000000000000, 0.000000000000000000, 0.000000000000000000 ) ) ;
#10819 = EDGE_CURVE ( 'NONE', #5404, #10823, #3211, .T. ) ;
#10820 = CARTESIAN_POINT ( 'NONE',  ( 4.212679447664376298, 6.814025269448777955, 3.747395293195558847E-16 ) ) ;
#10821 = FACE_OUTER_BOUND ( 'NONE', #9300, .T. ) ;
#10822 = CARTESIAN_POINT ( 'NONE',  ( 3.000000000000000888, -22.37663021667341923, -2.811977935938010376 ) ) ;
#10823 = VERTEX_POINT ( 'NONE', #5413 ) ;
#10824 = VERTEX_POINT ( 'NONE', #9199 ) ;
#10825 = CARTESIAN_POINT ( 'NONE',  ( -10.84705874452746777, 6.751620637726422736, 10.00000000000000000 ) ) ;
#10826 = VERTEX_POINT ( 'NONE', #4557 ) ;
#10827 = CARTESIAN_POINT ( 'NONE',  ( 0.07364157424580680678, -3.751631698233684364, 10.00000000000000000 ) ) ;
#10828 = DIRECTION ( 'NONE',  ( 1.000000000000000000, 0.000000000000000000, 0.000000000000000000 ) ) ;
#10829 = DIRECTION ( 'NONE',  ( 1.000000000000000000, 0.000000000000000000, -0.000000000000000000 ) ) ;
#10830 = AXIS2_PLACEMENT_3D ( 'NONE', #8906, #7051, #7112 ) ;
#10831 = DIRECTION ( 'NONE',  ( 0.000000000000000000, 0.000000000000000000, 1.000000000000000000 ) ) ;
#10832 = ORIENTED_EDGE ( 'NONE', *, *, #1917, .T. ) ;
#10833 = CARTESIAN_POINT ( 'NONE',  ( 0.000000000000000000, 17.35216073792440739, 17.71842311621536226 ) ) ;
#10834 = DIRECTION ( 'NONE',  ( 0.000000000000000000, 0.000000000000000000, 1.000000000000000000 ) ) ;
#10835 = CARTESIAN_POINT ( 'NONE',  ( 4.451863640887384399, 11.26298505921345594, 6.857782953271941950E-17 ) ) ;
#10836 = DIRECTION ( 'NONE',  ( 0.000000000000000000, 0.000000000000000000, -1.000000000000000000 ) ) ;
#10837 = AXIS2_PLACEMENT_3D ( 'NONE', #8593, #190, #10 ) ;
#10838 = CARTESIAN_POINT ( 'NONE',  ( 3.000000000000000888, -21.58580335785681115, 6.532525787310899723 ) ) ;
#10839 = ORIENTED_EDGE ( 'NONE', *, *, #8948, .T. ) ;
#10840 = EDGE_CURVE ( 'NONE', #7059, #1167, #7099, .T. ) ;
#10841 = CARTESIAN_POINT ( 'NONE',  ( 9.640149279600557009, 4.768118462334745011, 10.00000000000000000 ) ) ;
#10842 = CARTESIAN_POINT ( 'NONE',  ( 0.000000000000000000, -8.645255683529166291, 23.24434456306322971 ) ) ;
#10843 = DIRECTION ( 'NONE',  ( 0.000000000000000000, 0.1045284632676538872, -0.9945218953682732899 ) ) ;
#10844 = EDGE_LOOP ( 'NONE', ( #8436, #5613, #4864, #1991 ) ) ;
#10845 = AXIS2_PLACEMENT_3D ( 'NONE', #5637, #8396, #2829 ) ;
#10846 = EDGE_CURVE ( 'NONE', #11972, #5818, #3017, .T. ) ;
#10847 = DIRECTION ( 'NONE',  ( -1.000000000000000000, 0.000000000000000000, 0.000000000000000000 ) ) ;
#10848 = FACE_OUTER_BOUND ( 'NONE', #1043, .T. ) ;
#10849 = CARTESIAN_POINT ( 'NONE',  ( 5.893263639827395650, 6.717612500730409941, 10.00000000000000000 ) ) ;
#10850 = DIRECTION ( 'NONE',  ( -1.000000000000000000, 0.000000000000000000, 0.000000000000000000 ) ) ;
#10851 = CARTESIAN_POINT ( 'NONE',  ( 11.62709622633471618, -6.461356448465071622, 3.747395293195558847E-16 ) ) ;
#10852 = ADVANCED_FACE ( 'NONE', ( #11045 ), #3696, .T. ) ;
#10853 = CARTESIAN_POINT ( 'NONE',  ( 0.000000000000000000, -0.4575788569250363036, -22.54798042742718778 ) ) ;
#10854 = ORIENTED_EDGE ( 'NONE', *, *, #10619, .F. ) ;
#10855 = DIRECTION ( 'NONE',  ( 0.000000000000000000, 0.000000000000000000, 1.000000000000000000 ) ) ;
#10856 = EDGE_CURVE ( 'NONE', #4242, #9539, #1795, .T. ) ;
#10857 = ORIENTED_EDGE ( 'NONE', *, *, #2725, .T. ) ;
#10858 = ADVANCED_FACE ( 'NONE', ( #1623 ), #11832, .T. ) ;
#10859 = CARTESIAN_POINT ( 'NONE',  ( 3.000000000000000888, -18.40266524480597710, 13.79477846460790147 ) ) ;
#10860 = CARTESIAN_POINT ( 'NONE',  ( 0.000000000000000000, 24.45282072769606430, -4.135161237383341515 ) ) ;
#10861 =( NAMED_UNIT ( * ) PLANE_ANGLE_UNIT ( ) SI_UNIT ( $, .RADIAN. ) );
#10862 = ORIENTED_EDGE ( 'NONE', *, *, #9914, .T. ) ;
#10863 = DIRECTION ( 'NONE',  ( -1.000000000000000000, 0.000000000000000000, -0.000000000000000000 ) ) ;
#10864 = CARTESIAN_POINT ( 'NONE',  ( 3.000000000000000888, -22.37663021667341923, 6.788022064061986605 ) ) ;
#10865 = CARTESIAN_POINT ( 'NONE',  ( 0.000000000000000000, 15.13242714128143440, -17.31945870441131419 ) ) ;
#10866 = CIRCLE ( 'NONE', #6934, 18.49999999999999645 ) ;
#10867 = CARTESIAN_POINT ( 'NONE',  ( -2.764021070441483374, -10.29567250283335689, 6.857782953271941950E-17 ) ) ;
#10868 = DIRECTION ( 'NONE',  ( 1.000000000000000000, 0.000000000000000000, 0.000000000000000000 ) ) ;
#10869 = FACE_OUTER_BOUND ( 'NONE', #5302, .T. ) ;
#10870 = EDGE_LOOP ( 'NONE', ( #6872, #1396, #3243, #9095 ) ) ;
#10871 = VERTEX_POINT ( 'NONE', #5291 ) ;
#10872 = VERTEX_POINT ( 'NONE', #5359 ) ;
#10873 = CIRCLE ( 'NONE', #5005, 9.599999999999996092 ) ;
#10874 = CARTESIAN_POINT ( 'NONE',  ( 5.172292865810427465, -11.91455349003027919, 10.00000000000000000 ) ) ;
#10875 = CARTESIAN_POINT ( 'NONE',  ( 0.000000000000000000, 0.000000000000000000, 0.000000000000000000 ) ) ;
#10876 = DIRECTION ( 'NONE',  ( -1.000000000000000000, -0.000000000000000000, -0.000000000000000000 ) ) ;
#10877 = CARTESIAN_POINT ( 'NONE',  ( -4.763935748648512991, -4.221771024091821367, 3.747395293195558847E-16 ) ) ;
#10878 = EDGE_CURVE ( 'NONE', #2308, #6849, #4576, .T. ) ;
#10879 = DIRECTION ( 'NONE',  ( 8.673617379884035472E-16, 1.000000000000000000, 0.000000000000000000 ) ) ;
#10880 = CIRCLE ( 'NONE', #8536, 3.500000000000000000 ) ;
#10881 = CYLINDRICAL_SURFACE ( 'NONE', #1745, 9.599999999999997868 ) ;
#10882 = ORIENTED_EDGE ( 'NONE', *, *, #4948, .F. ) ;
#10883 = EDGE_LOOP ( 'NONE', ( #8418, #2998 ) ) ;
#10884 = ORIENTED_EDGE ( 'NONE', *, *, #11256, .T. ) ;
#10885 = CARTESIAN_POINT ( 'NONE',  ( 4.321204520403006732, 2.017656881711013206, 10.00000000000000000 ) ) ;
#10886 = FACE_OUTER_BOUND ( 'NONE', #9525, .T. ) ;
#10887 = CARTESIAN_POINT ( 'NONE',  ( 3.000000000000000888, 18.40266524480588473, 13.79477846460802226 ) ) ;
#10888 = EDGE_CURVE ( 'NONE', #6277, #6987, #2422, .T. ) ;
#10889 = CARTESIAN_POINT ( 'NONE',  ( 3.000000000000000888, 11.20082935824075321, 20.08719549084868561 ) ) ;
#10890 = ORIENTED_EDGE ( 'NONE', *, *, #9164, .F. ) ;
#10891 = CARTESIAN_POINT ( 'NONE',  ( 3.000000000000000888, -0.4575788569250363036, -22.54798042742718778 ) ) ;
#10892 = CARTESIAN_POINT ( 'NONE',  ( 0.000000000000000000, -22.37663021667346186, 2.811977935937707063 ) ) ;
#10893 = CARTESIAN_POINT ( 'NONE',  ( -1.672018190274121574, 9.216430685901386255, 6.857782953271941950E-17 ) ) ;
#10894 = FACE_OUTER_BOUND ( 'NONE', #9079, .T. ) ;
#10895 = CARTESIAN_POINT ( 'NONE',  ( 8.000000000000000000, 2.265596578422603002E-15, -18.49999999999999645 ) ) ;
#10896 = EDGE_LOOP ( 'NONE', ( #4597, #1470, #5676, #3074 ) ) ;
#10897 = VECTOR ( 'NONE', #2289, 1000.000000000000000 ) ;
#10898 = CARTESIAN_POINT ( 'NONE',  ( -5.319913005755715574, -3.351504787099933047, 10.00000000000000000 ) ) ;
#10899 = ORIENTED_EDGE ( 'NONE', *, *, #9453, .T. ) ;
#10900 = DIRECTION ( 'NONE',  ( 0.000000000000000000, 0.9135454576426018658, -0.4067366430757979323 ) ) ;
#10901 = LINE ( 'NONE', #7153, #7771 ) ;
#10902 = CARTESIAN_POINT ( 'NONE',  ( 3.000000000000000888, 0.000000000000000000, 0.000000000000000000 ) ) ;
#10903 = CARTESIAN_POINT ( 'NONE',  ( 6.689389171169565884, -4.795626085247176817, 10.00000000000000000 ) ) ;
#10904 = CIRCLE ( 'NONE', #8169, 9.599999999999997868 ) ;
#10905 = DIRECTION ( 'NONE',  ( -1.000000000000000000, 0.000000000000000000, -0.000000000000000000 ) ) ;
#10906 = CYLINDRICAL_SURFACE ( 'NONE', #6074, 9.599999999999997868 ) ;
#10907 = ORIENTED_EDGE ( 'NONE', *, *, #4570, .T. ) ;
#10908 = CARTESIAN_POINT ( 'NONE',  ( 3.000000000000000888, -17.06259499759935139, -14.74749645580028101 ) ) ;
#10909 = ORIENTED_EDGE ( 'NONE', *, *, #8689, .T. ) ;
#10910 = CARTESIAN_POINT ( 'NONE',  ( 4.321204520403003180, 2.017656881711011430, 3.747395293195558847E-16 ) ) ;
#10911 = AXIS2_PLACEMENT_3D ( 'NONE', #5792, #1929, #3889 ) ;
#10912 = DIRECTION ( 'NONE',  ( 0.000000000000000000, 0.000000000000000000, 1.000000000000000000 ) ) ;
#10913 = ORIENTED_EDGE ( 'NONE', *, *, #9683, .F. ) ;
#10914 = FACE_OUTER_BOUND ( 'NONE', #3885, .T. ) ;
#10915 = EDGE_CURVE ( 'NONE', #7882, #139, #75, .T. ) ;
#10916 = DIRECTION ( 'NONE',  ( -1.000000000000000000, -0.000000000000000000, -0.000000000000000000 ) ) ;
#10917 = CARTESIAN_POINT ( 'NONE',  ( -2.570438583093578533, 5.934334910739571534, 10.00000000000000000 ) ) ;
#10919 = EDGE_CURVE ( 'NONE', #4735, #5828, #8351, .T. ) ;
#10918 = CARTESIAN_POINT ( 'NONE',  ( -0.1814876354083659327, -10.77628937513454943, 6.857782953271941950E-17 ) ) ;
#10920 = LINE ( 'NONE', #2537, #3555 ) ;
#10921 = EDGE_CURVE ( 'NONE', #11050, #7635, #10046, .T. ) ;
#10922 = VECTOR ( 'NONE', #9719, 1000.000000000000000 ) ;
#10923 = DIRECTION ( 'NONE',  ( -1.000000000000000000, -0.000000000000000000, -0.000000000000000000 ) ) ;
#10924 = EDGE_LOOP ( 'NONE', ( #6426, #5335, #11931, #11248 ) ) ;
#10925 = ORIENTED_EDGE ( 'NONE', *, *, #4237, .T. ) ;
#10926 = ORIENTED_EDGE ( 'NONE', *, *, #12072, .F. ) ;
#10927 = CARTESIAN_POINT ( 'NONE',  ( -11.99326810842507562, 8.590522060507204571, 10.00000000000000000 ) ) ;
#10929 = ADVANCED_FACE ( 'NONE', ( #6338 ), #7292, .T. ) ;
#10928 = AXIS2_PLACEMENT_3D ( 'NONE', #8130, #8069, #7136 ) ;
#10930 = AXIS2_PLACEMENT_3D ( 'NONE', #3312, #8375, #1885 ) ;
#10931 = FACE_OUTER_BOUND ( 'NONE', #11959, .T. ) ;
#10932 = CARTESIAN_POINT ( 'NONE',  ( 0.000000000000000000, 1.039229259764835600, -24.77821629063820907 ) ) ;
#10933 = CARTESIAN_POINT ( 'NONE',  ( -0.1881845630465192321, -6.755137126427047001, 3.747395293195558847E-16 ) ) ;
#10934 = DIRECTION ( 'NONE',  ( -1.000000000000000000, -0.000000000000000000, -0.000000000000000000 ) ) ;
#10935 = CIRCLE ( 'NONE', #3318, 9.599999999999996092 ) ;
#10936 = CARTESIAN_POINT ( 'NONE',  ( 0.000000000000000000, -13.62355943574006645, -17.97274125076088680 ) ) ;
#10937 = ORIENTED_EDGE ( 'NONE', *, *, #7263, .T. ) ;
#10938 = EDGE_LOOP ( 'NONE', ( #6422, #4927, #7505, #266 ) ) ;
#10939 = EDGE_CURVE ( 'NONE', #6849, #6658, #639, .T. ) ;
#10940 = CONTEXT_DEPENDENT_SHAPE_REPRESENTATION ( #3244, #5707 ) ;
#10941 = ORIENTED_EDGE ( 'NONE', *, *, #7874, .T. ) ;
#10942 = DIRECTION ( 'NONE',  ( -1.000000000000000000, -0.000000000000000000, 0.000000000000000000 ) ) ;
#10943 = CARTESIAN_POINT ( 'NONE',  ( -10.00000000000000000, 0.000000000000000000, 0.000000000000000000 ) ) ;
#10944 = ADVANCED_FACE ( 'NONE', ( #11950 ), #6447, .T. ) ;
#10945 = CARTESIAN_POINT ( 'NONE',  ( 1.500000000000000222, 0.000000000000000000, 0.000000000000000000 ) ) ;
#10946 = ORIENTED_EDGE ( 'NONE', *, *, #2052, .F. ) ;
#10947 = FACE_BOUND ( 'NONE', #10499, .T. ) ;
#10948 = VECTOR ( 'NONE', #2049, 1000.000000000000000 ) ;
#10949 = CARTESIAN_POINT ( 'NONE',  ( 11.50000000000000178, 1.408343819019456373E-15, 3.000000000000000000 ) ) ;
#10950 = CARTESIAN_POINT ( 'NONE',  ( 3.666996827460249797, 4.772409917195337137, 6.857782953271941950E-17 ) ) ;
#10951 = EDGE_CURVE ( 'NONE', #4817, #11323, #10637, .T. ) ;
#10952 = CARTESIAN_POINT ( 'NONE',  ( 3.000000000000000888, 22.37663021667344054, -2.811977935937859385 ) ) ;
#10953 = ORIENTED_EDGE ( 'NONE', *, *, #71, .T. ) ;
#10954 = DIRECTION ( 'NONE',  ( 0.000000000000000000, -0.9945218953682744001, 0.1045284632676436593 ) ) ;
#10955 = AXIS2_PLACEMENT_3D ( 'NONE', #1611, #3389, #11876 ) ;
#10956 = ORIENTED_EDGE ( 'NONE', *, *, #299, .T. ) ;
#10957 = ORIENTED_EDGE ( 'NONE', *, *, #9648, .F. ) ;
#10958 = AXIS2_PLACEMENT_3D ( 'NONE', #6480, #4403, #5388 ) ;
#10959 = CARTESIAN_POINT ( 'NONE',  ( -5.862605222286289219, -1.923479314576678423, 10.00000000000000000 ) ) ;
#10960 = AXIS2_PLACEMENT_3D ( 'NONE', #6616, #6558, #1722 ) ;
#10961 = ORIENTED_EDGE ( 'NONE', *, *, #5184, .F. ) ;
#10962 = CARTESIAN_POINT ( 'NONE',  ( 3.000000000000000888, -22.37663021667341923, -2.811977935938010376 ) ) ;
#10963 =( GEOMETRIC_REPRESENTATION_CONTEXT ( 3 ) GLOBAL_UNCERTAINTY_ASSIGNED_CONTEXT ( ( #852 ) ) GLOBAL_UNIT_ASSIGNED_CONTEXT ( ( #3873, #7480, #10696 ) ) REPRESENTATION_CONTEXT ( 'NONE', 'WORKASPACE' ) );
#10964 = ORIENTED_EDGE ( 'NONE', *, *, #10248, .T. ) ;
#10965 = DIRECTION ( 'NONE',  ( 0.000000000000000000, 0.000000000000000000, 1.000000000000000000 ) ) ;
#10966 = DIRECTION ( 'NONE',  ( 1.000000000000000000, 0.000000000000000000, -0.000000000000000000 ) ) ;
#10967 = CARTESIAN_POINT ( 'NONE',  ( 2.469054641153702434, -10.61194774715159994, 10.00000000000000000 ) ) ;
#10968 = CIRCLE ( 'NONE', #7239, 24.80000000000000071 ) ;
#10969 = CARTESIAN_POINT ( 'NONE',  ( 3.000000000000000888, 11.67026512804547345, 19.29833442572363822 ) ) ;
#10970 = EDGE_CURVE ( 'NONE', #9017, #2317, #2822, .T. ) ;
#10971 = CARTESIAN_POINT ( 'NONE',  ( 3.000000000000000888, 19.75591328264886215, 10.87771529938168946 ) ) ;
#10972 = VERTEX_POINT ( 'NONE', #1918 ) ;
#10973 = ORIENTED_EDGE ( 'NONE', *, *, #7854, .T. ) ;
#10974 = CARTESIAN_POINT ( 'NONE',  ( 3.000000000000000888, -21.58580335785672233, -6.532525787311189269 ) ) ;
#10975 = VERTEX_POINT ( 'NONE', #11405 ) ;
#10976 = CARTESIAN_POINT ( 'NONE',  ( -1.784247137544765716, 5.123456263349895679, 3.747395293195558847E-16 ) ) ;
#10977 = AXIS2_PLACEMENT_3D ( 'NONE', #8537, #9629, #3945 ) ;
#10978 = AXIS2_PLACEMENT_3D ( 'NONE', #1378, #5111, #8854 ) ;
#10979 = DIRECTION ( 'NONE',  ( 0.000000000000000000, 0.000000000000000000, 1.000000000000000000 ) ) ;
#10980 =( LENGTH_UNIT ( ) NAMED_UNIT ( * ) SI_UNIT ( .MILLI., .METRE. ) );
#10981 = ORIENTED_EDGE ( 'NONE', *, *, #9789, .F. ) ;
#10982 = AXIS2_PLACEMENT_3D ( 'NONE', #1860, #7418, #5536 ) ;
#10983 = CYLINDRICAL_SURFACE ( 'NONE', #930, 9.599999999999997868 ) ;
#10984 = CARTESIAN_POINT ( 'NONE',  ( 3.000000000000000888, -19.74380051311532114, -11.79560690673893042 ) ) ;
#10985 = CARTESIAN_POINT ( 'NONE',  ( -6.191802569540381995, -3.848120238388911041, 10.00000000000000000 ) ) ;
#10986 = CARTESIAN_POINT ( 'NONE',  ( 5.531377455021717182, -0.3672033614207537711, 6.857782953271941950E-17 ) ) ;
#10987 = DIRECTION ( 'NONE',  ( -1.000000000000000000, -0.000000000000000000, -0.000000000000000000 ) ) ;
#10988 = CARTESIAN_POINT ( 'NONE',  ( 0.000000000000000000, 19.43515443678423793, -15.40502424595125852 ) ) ;
#10989 = CIRCLE ( 'NONE', #3372, 22.99899999999999523 ) ;
#10990 = ORIENTED_EDGE ( 'NONE', *, *, #825, .F. ) ;
#10991 = AXIS2_PLACEMENT_3D ( 'NONE', #4650, #2631, #9239 ) ;
#10992 = APPLICATION_CONTEXT ( 'automotive_design' ) ;
#10993 = ORIENTED_EDGE ( 'NONE', *, *, #5608, .F. ) ;
#10994 = EDGE_LOOP ( 'NONE', ( #961, #340, #4893, #11926 ) ) ;
#10995 = CARTESIAN_POINT ( 'NONE',  ( -3.043536693350107569, 14.07442491708026111, 10.00000000000000000 ) ) ;
#10996 = EDGE_CURVE ( 'NONE', #10809, #10316, #6914, .T. ) ;
#10997 = CIRCLE ( 'NONE', #9823, 9.599999999999999645 ) ;
#10998 = CARTESIAN_POINT ( 'NONE',  ( 0.000000000000000000, 0.000000000000000000, 0.000000000000000000 ) ) ;
#10999 = DIRECTION ( 'NONE',  ( -1.000000000000000000, -0.000000000000000000, -0.000000000000000000 ) ) ;
#11000 = ADVANCED_FACE ( 'NONE', ( #2966 ), #6625, .T. ) ;
#11001 = CARTESIAN_POINT ( 'NONE',  ( 5.657123057053811799, 5.504982807385217392, 3.747395293195558847E-16 ) ) ;
#11002 = CARTESIAN_POINT ( 'NONE',  ( 3.000000000000000888, 0.000000000000000000, 0.000000000000000000 ) ) ;
#11003 = EDGE_CURVE ( 'NONE', #3932, #6844, #7898, .T. ) ;
#11004 = CARTESIAN_POINT ( 'NONE',  ( 1.499999999999999556, 24.75110766671652129, 1.556492618230721492 ) ) ;
#11005 = EDGE_LOOP ( 'NONE', ( #2772, #1789 ) ) ;
#11006 = AXIS2_PLACEMENT_3D ( 'NONE', #1844, #8395, #987 ) ;
#11007 = ORIENTED_EDGE ( 'NONE', *, *, #5841, .T. ) ;
#11008 = EDGE_CURVE ( 'NONE', #1640, #8914, #8876, .T. ) ;
#11009 = ORIENTED_EDGE ( 'NONE', *, *, #875, .T. ) ;
#11010 = CARTESIAN_POINT ( 'NONE',  ( -0.9167995209625440234, 5.268308710424125074, 10.00000000000000000 ) ) ;
#11011 = VECTOR ( 'NONE', #1643, 1000.000000000000000 ) ;
#11012 = AXIS2_PLACEMENT_3D ( 'NONE', #9268, #2845, #887 ) ;
#11013 = CARTESIAN_POINT ( 'NONE',  ( 3.000000000000000888, -6.532525787311115550, 21.58580335785674365 ) ) ;
#11014 = DIRECTION ( 'NONE',  ( -1.000000000000000000, 0.000000000000000000, -0.000000000000000000 ) ) ;
#11015 = CIRCLE ( 'NONE', #6905, 24.80000000000000071 ) ;
#11016 = DIRECTION ( 'NONE',  ( 0.000000000000000000, -0.9135454576425964257, -0.4067366430758104223 ) ) ;
#11017 = DIRECTION ( 'NONE',  ( -1.000000000000000000, -0.000000000000000000, -0.000000000000000000 ) ) ;
#11018 = CARTESIAN_POINT ( 'NONE',  ( 4.503282398433332112, -2.806195971666638922, 6.857782953271941950E-17 ) ) ;
#11019 = DIRECTION ( 'NONE',  ( -1.000000000000000000, 0.000000000000000000, -0.000000000000000000 ) ) ;
#11020 = ORIENTED_EDGE ( 'NONE', *, *, #9726, .F. ) ;
#11021 = DIRECTION ( 'NONE',  ( 0.000000000000000000, -0.9510565162951504226, -0.3090169943749574433 ) ) ;
#11022 = ORIENTED_EDGE ( 'NONE', *, *, #1982, .F. ) ;
#11023 = AXIS2_PLACEMENT_3D ( 'NONE', #45, #1093, #12040 ) ;
#11024 = CARTESIAN_POINT ( 'NONE',  ( -5.704017324792772570, 1.489539271746576743, 10.00000000000000000 ) ) ;
#11025 = ORIENTED_EDGE ( 'NONE', *, *, #7199, .T. ) ;
#11026 = DIRECTION ( 'NONE',  ( -1.000000000000000000, 0.000000000000000000, 0.000000000000000000 ) ) ;
#11027 = VERTEX_POINT ( 'NONE', #10482 ) ;
#11028 = CARTESIAN_POINT ( 'NONE',  ( 3.000000000000000888, 9.039786367039127413, -21.14796121233187520 ) ) ;
#11029 = CARTESIAN_POINT ( 'NONE',  ( 3.000000000000000888, 9.589108953447894379, 20.41249101028215307 ) ) ;
#11030 = CARTESIAN_POINT ( 'NONE',  ( 13.67726327739689829, -10.50289975150003485, 6.857782953271941950E-17 ) ) ;
#11031 = AXIS2_PLACEMENT_3D ( 'NONE', #2779, #4490, #820 ) ;
#11032 = CARTESIAN_POINT ( 'NONE',  ( 3.000000000000000888, 20.86861857134734421, 9.667200211209893368 ) ) ;
#11033 = EDGE_CURVE ( 'NONE', #3365, #4516, #9665, .T. ) ;
#11034 = FACE_OUTER_BOUND ( 'NONE', #9047, .T. ) ;
#11035 = EDGE_LOOP ( 'NONE', ( #3526, #4406, #459, #681 ) ) ;
#11036 = ORIENTED_EDGE ( 'NONE', *, *, #11363, .F. ) ;
#11037 = CARTESIAN_POINT ( 'NONE',  ( 3.000000000000000888, 22.56530478845654386, -4.445336973060635799 ) ) ;
#11038 = ORIENTED_EDGE ( 'NONE', *, *, #6335, .T. ) ;
#11039 = CARTESIAN_POINT ( 'NONE',  ( 16.50000000000000355, 0.000000000000000000, 10.00000000000000000 ) ) ;
#11040 = AXIS2_PLACEMENT_3D ( 'NONE', #4741, #7667, #258 ) ;
#11041 = LINE ( 'NONE', #9192, #11835 ) ;
#11042 = SURFACE_STYLE_FILL_AREA ( #6205 ) ;
#11043 = EDGE_CURVE ( 'NONE', #4836, #10397, #5562, .T. ) ;
#11044 = CARTESIAN_POINT ( 'NONE',  ( 3.000000000000000888, -13.28910708463142498, 20.93895013827577145 ) ) ;
#11045 = FACE_OUTER_BOUND ( 'NONE', #426, .T. ) ;
#11046 = CARTESIAN_POINT ( 'NONE',  ( -14.12277927129996158, -8.146689865454478152, 10.00000000000000000 ) ) ;
#11047 = CARTESIAN_POINT ( 'NONE',  ( 5.312937634499088624, -1.259815497212412261, 6.857782953271941950E-17 ) ) ;
#11048 = DIRECTION ( 'NONE',  ( 0.000000000000000000, 0.000000000000000000, -1.000000000000000000 ) ) ;
#11049 = CARTESIAN_POINT ( 'NONE',  ( 3.000000000000000888, 11.67026512804572924, -19.29833442572348190 ) ) ;
#11050 = VERTEX_POINT ( 'NONE', #8411 ) ;
#11051 = ORIENTED_EDGE ( 'NONE', *, *, #6795, .T. ) ;
#11052 = CARTESIAN_POINT ( 'NONE',  ( 13.24268851590354146, -2.403973981685017414, 10.00000000000000000 ) ) ;
#11053 = CARTESIAN_POINT ( 'NONE',  ( 0.000000000000000000, 0.000000000000000000, -15.00000000000000000 ) ) ;
#11054 = DIRECTION ( 'NONE',  ( -1.000000000000000000, 0.000000000000000000, -0.000000000000000000 ) ) ;
#11055 = AXIS2_PLACEMENT_3D ( 'NONE', #1550, #6682, #9380 ) ;
#11056 = CARTESIAN_POINT ( 'NONE',  ( 2.084958754360775934, -3.480815169281481047, 3.747395293195558847E-16 ) ) ;
#11057 = DIRECTION ( 'NONE',  ( -1.000000000000000000, -0.000000000000000000, -0.000000000000000000 ) ) ;
#11058 = ORIENTED_EDGE ( 'NONE', *, *, #11459, .T. ) ;
#11059 = DIRECTION ( 'NONE',  ( 0.000000000000000000, -0.9781476007338034684, -0.2079116908177697509 ) ) ;
#11060 = ORIENTED_EDGE ( 'NONE', *, *, #6432, .T. ) ;
#11061 = VERTEX_POINT ( 'NONE', #7483 ) ;
#11062 = DIRECTION ( 'NONE',  ( 0.000000000000000000, 0.000000000000000000, 1.000000000000000000 ) ) ;
#11063 = EDGE_CURVE ( 'NONE', #862, #3166, #1859, .T. ) ;
#11064 = DIRECTION ( 'NONE',  ( 0.000000000000000000, 0.3090169943749480064, -0.9510565162951533091 ) ) ;
#11065 = LINE ( 'NONE', #8192, #9119 ) ;
#11066 = PRODUCT_RELATED_PRODUCT_CATEGORY ( 'part', '', ( #2185 ) ) ;
#11067 = DIRECTION ( 'NONE',  ( -1.000000000000000000, -0.000000000000000000, -0.000000000000000000 ) ) ;
#11068 = AXIS2_PLACEMENT_3D ( 'NONE', #5577, #1161, #8460 ) ;
#11069 = ADVANCED_FACE ( 'NONE', ( #5593 ), #9382, .T. ) ;
#11070 = DIRECTION ( 'NONE',  ( 0.000000000000000000, -0.2079116908177466305, -0.9781476007338082423 ) ) ;
#11071 = LINE ( 'NONE', #10681, #7449 ) ;
#11072 = EDGE_CURVE ( 'NONE', #10781, #5937, #9503, .T. ) ;
#11073 = FACE_OUTER_BOUND ( 'NONE', #5558, .T. ) ;
#11074 = EDGE_LOOP ( 'NONE', ( #11304, #7507, #1235, #8665 ) ) ;
#11075 = ORIENTED_EDGE ( 'NONE', *, *, #2355, .F. ) ;
#11076 = FACE_OUTER_BOUND ( 'NONE', #4832, .T. ) ;
#11077 = EDGE_LOOP ( 'NONE', ( #6381, #3470, #2618, #917 ) ) ;
#11078 = ORIENTED_EDGE ( 'NONE', *, *, #101, .F. ) ;
#11079 = CARTESIAN_POINT ( 'NONE',  ( -5.962113107391272315, -1.426310550302921865, 10.00000000000000000 ) ) ;
#11080 = EDGE_LOOP ( 'NONE', ( #10151, #935, #12051, #7326 ) ) ;
#11081 = DIRECTION ( 'NONE',  ( 0.000000000000000000, -0.9135454576426046414, 0.4067366430757920481 ) ) ;
#11082 = ORIENTED_EDGE ( 'NONE', *, *, #4345, .T. ) ;
#11083 = ADVANCED_FACE ( 'NONE', ( #5723 ), #3762, .T. ) ;
#11084 = DIRECTION ( 'NONE',  ( -1.000000000000000000, -0.000000000000000000, 0.000000000000000000 ) ) ;
#11085 = CARTESIAN_POINT ( 'NONE',  ( 1.500000000000000444, -17.35216073792452107, 17.71842311621524146 ) ) ;
#11086 = CARTESIAN_POINT ( 'NONE',  ( 4.346347989804005607, 4.041826679702273495, 10.00000000000000000 ) ) ;
#11087 = DIRECTION ( 'NONE',  ( -1.000000000000000000, 0.000000000000000000, 0.000000000000000000 ) ) ;
#11088 = CARTESIAN_POINT ( 'NONE',  ( 0.000000000000000000, 22.83456483164689033, 2.745295967526073078 ) ) ;
#11089 = ORIENTED_EDGE ( 'NONE', *, *, #5774, .F. ) ;
#11090 = LINE ( 'NONE', #2706, #3725 ) ;
#11091 = ORIENTED_EDGE ( 'NONE', *, *, #11991, .T. ) ;
#11092 = ADVANCED_FACE ( 'NONE', ( #3943 ), #1007, .T. ) ;
#11093 = CARTESIAN_POINT ( 'NONE',  ( -4.763935748648512991, -4.221771024091821367, 3.747395293195558847E-16 ) ) ;
#11094 = VECTOR ( 'NONE', #9577, 1000.000000000000000 ) ;
#11095 = CARTESIAN_POINT ( 'NONE',  ( 0.000000000000000000, 0.000000000000000000, 0.000000000000000000 ) ) ;
#11096 = EDGE_CURVE ( 'NONE', #4186, #5315, #3810, .T. ) ;
#11097 = FACE_OUTER_BOUND ( 'NONE', #3287, .T. ) ;
#11098 = CYLINDRICAL_SURFACE ( 'NONE', #8242, 22.99899999999999878 ) ;
#11099 = CARTESIAN_POINT ( 'NONE',  ( 3.000000000000000888, 20.41249101028211754, -9.589108953447965433 ) ) ;
#11100 = CARTESIAN_POINT ( 'NONE',  ( 0.000000000000000000, 0.000000000000000000, 0.000000000000000000 ) ) ;
#11101 = CARTESIAN_POINT ( 'NONE',  ( 8.235329212250112718, -1.783486464602660027, 6.857782953271941950E-17 ) ) ;
#11102 = DIRECTION ( 'NONE',  ( 0.000000000000000000, 0.7431448254773909134, 0.6691306063588619013 ) ) ;
#11103 = DIRECTION ( 'NONE',  ( -1.000000000000000000, -0.000000000000000000, 0.000000000000000000 ) ) ;
#11104 = ORIENTED_EDGE ( 'NONE', *, *, #8498, .T. ) ;
#11105 = EDGE_CURVE ( 'NONE', #10471, #6735, #3418, .T. ) ;
#11106 = ORIENTED_EDGE ( 'NONE', *, *, #10919, .T. ) ;
#11107 = EDGE_LOOP ( 'NONE', ( #675, #4637, #4566, #1776 ) ) ;
#11108 = DIRECTION ( 'NONE',  ( 0.000000000000000000, 0.5877852522924742473, -0.8090169943749467851 ) ) ;
#11109 = CARTESIAN_POINT ( 'NONE',  ( 7.316052646047090491, -7.060001943526881263, 10.00000000000000000 ) ) ;
#11110 = LINE ( 'NONE', #707, #1925 ) ;
#11111 = DIRECTION ( 'NONE',  ( 1.000000000000000000, 0.000000000000000000, 0.000000000000000000 ) ) ;
#11112 = CARTESIAN_POINT ( 'NONE',  ( 3.656769781543557141, 7.172433557890304456, 3.747395293195558847E-16 ) ) ;
#11113 = CIRCLE ( 'NONE', #4872, 18.49999999999999645 ) ;
#11114 = VECTOR ( 'NONE', #7693, 1000.000000000000000 ) ;
#11115 = LINE ( 'NONE', #7370, #8062 ) ;
#11116 = DIRECTION ( 'NONE',  ( 1.000000000000000000, 0.000000000000000000, 0.000000000000000000 ) ) ;
#11117 = ORIENTED_EDGE ( 'NONE', *, *, #3784, .F. ) ;
#11118 = ORIENTED_EDGE ( 'NONE', *, *, #6179, .F. ) ;
#11119 = ORIENTED_EDGE ( 'NONE', *, *, #8776, .F. ) ;
#11120 = DIRECTION ( 'NONE',  ( -1.000000000000000000, -0.000000000000000000, 0.000000000000000000 ) ) ;
#11121 = PRESENTATION_LAYER_ASSIGNMENT (  '', '', ( #9368 ) ) ;
#11122 = CARTESIAN_POINT ( 'NONE',  ( 3.000000000000000888, 15.40502424595145037, 19.43515443678408516 ) ) ;
#11123 = DIRECTION ( 'NONE',  ( -1.000000000000000000, 0.000000000000000000, 0.000000000000000000 ) ) ;
#11124 = FACE_OUTER_BOUND ( 'NONE', #19, .T. ) ;
#11125 = DIRECTION ( 'NONE',  ( -1.000000000000000000, 0.000000000000000000, 0.000000000000000000 ) ) ;
#11126 = CARTESIAN_POINT ( 'NONE',  ( 13.03626601087042758, 4.193914020170396384, 3.747395293195558847E-16 ) ) ;
#11127 = CARTESIAN_POINT ( 'NONE',  ( -6.825012239887737309, 1.243808647927286515, 6.857782953271941950E-17 ) ) ;
#11128 = CIRCLE ( 'NONE', #6041, 22.99899999999999878 ) ;
#11129 = AXIS2_PLACEMENT_3D ( 'NONE', #4884, #8683, #156 ) ;
#11130 = AXIS2_PLACEMENT_3D ( 'NONE', #530, #1453, #5187 ) ;
#11131 = CARTESIAN_POINT ( 'NONE',  ( 3.000000000000000888, 22.37663021667340146, 2.811977935938166695 ) ) ;
#11132 = VERTEX_POINT ( 'NONE', #11463 ) ;
#11133 = VERTEX_POINT ( 'NONE', #941 ) ;
#11134 = DIRECTION ( 'NONE',  ( 1.000000000000000000, 0.000000000000000000, 0.000000000000000000 ) ) ;
#11135 = ORIENTED_EDGE ( 'NONE', *, *, #3182, .T. ) ;
#11136 = EDGE_LOOP ( 'NONE', ( #4089, #1935, #11592, #8105 ) ) ;
#11137 = CARTESIAN_POINT ( 'NONE',  ( 6.411932913581408044, 4.469049885107577502, 10.00000000000000000 ) ) ;
#11138 = EDGE_CURVE ( 'NONE', #1768, #1367, #6565, .T. ) ;
#11139 = ORIENTED_EDGE ( 'NONE', *, *, #7879, .T. ) ;
#11140 = CARTESIAN_POINT ( 'NONE',  ( 3.000000000000000888, -20.86861857134728027, -9.667200211210033700 ) ) ;
#11141 = EDGE_CURVE ( 'NONE', #2390, #1419, #3607, .T. ) ;
#11142 = EDGE_LOOP ( 'NONE', ( #435, #9066, #10041, #11995 ) ) ;
#11143 = ADVANCED_FACE ( 'NONE', ( #4797 ), #8533, .T. ) ;
#11144 = CIRCLE ( 'NONE', #6643, 9.599999999999997868 ) ;
#11145 = DIRECTION ( 'NONE',  ( -0.000000000000000000, -0.000000000000000000, 1.000000000000000000 ) ) ;
#11146 = APPLICATION_CONTEXT ( 'automotive_design' ) ;
#11147 = DIRECTION ( 'NONE',  ( 0.000000000000000000, -0.9945218953682744001, 0.1045284632676437564 ) ) ;
#11148 = CARTESIAN_POINT ( 'NONE',  ( 0.3111040546027374343, -4.780743156735979049, 10.00000000000000000 ) ) ;
#11149 = DIRECTION ( 'NONE',  ( -1.000000000000000000, 0.000000000000000000, 0.000000000000000000 ) ) ;
#11150 = AXIS2_PLACEMENT_3D ( 'NONE', #11346, #3032, #501 ) ;
#11151 = CARTESIAN_POINT ( 'NONE',  ( -4.500000000000000888, -0.5000000000000000000, 0.000000000000000000 ) ) ;
#11152 = ORIENTED_EDGE ( 'NONE', *, *, #2783, .T. ) ;
#11153 = ORIENTED_EDGE ( 'NONE', *, *, #846, .T. ) ;
#11154 = DIRECTION ( 'NONE',  ( -1.000000000000000000, -0.000000000000000000, -0.000000000000000000 ) ) ;
#11155 = CIRCLE ( 'NONE', #7031, 9.599999999999996092 ) ;
#11156 = ORIENTED_EDGE ( 'NONE', *, *, #3225, .F. ) ;
#11157 = EDGE_CURVE ( 'NONE', #762, #9917, #10440, .T. ) ;
#11158 = MECHANICAL_DESIGN_GEOMETRIC_PRESENTATION_REPRESENTATION (  '', ( #9786 ), #7631 ) ;
#11159 = CARTESIAN_POINT ( 'NONE',  ( -3.038216613429991053, 4.635879136410029133, 3.747395293195558847E-16 ) ) ;
#11160 = ADVANCED_FACE ( 'NONE', ( #316 ), #8892, .T. ) ;
#11161 = CARTESIAN_POINT ( 'NONE',  ( -1.500000000000000222, 1.836970198721030181E-16, 0.000000000000000000 ) ) ;
#11162 =( NAMED_UNIT ( * ) SI_UNIT ( $, .STERADIAN. ) SOLID_ANGLE_UNIT ( ) );
#11163 = ORIENTED_EDGE ( 'NONE', *, *, #8312, .T. ) ;
#11164 = LINE ( 'NONE', #1004, #2108 ) ;
#11165 = AXIS2_PLACEMENT_3D ( 'NONE', #727, #8264, #1895 ) ;
#11166 = CARTESIAN_POINT ( 'NONE',  ( 3.000000000000000888, 0.000000000000000000, 0.000000000000000000 ) ) ;
#11167 = FACE_OUTER_BOUND ( 'NONE', #8815, .T. ) ;
#11168 = CARTESIAN_POINT ( 'NONE',  ( 8.393308867179008814, -1.106660293010312213, 6.857782953271941950E-17 ) ) ;
#11169 = DIRECTION ( 'NONE',  ( -1.000000000000000000, 0.000000000000000000, -0.000000000000000000 ) ) ;
#11170 = CARTESIAN_POINT ( 'NONE',  ( 0.000000000000000000, 5.135568396240030253, 21.96011696265493285 ) ) ;
#11171 = DIRECTION ( 'NONE',  ( 0.000000000000000000, -0.9945218953682721796, -0.1045284632676635739 ) ) ;
#11172 = ORIENTED_EDGE ( 'NONE', *, *, #10846, .F. ) ;
#11173 = CIRCLE ( 'NONE', #8451, 22.99899999999999523 ) ;
#11174 = VERTEX_POINT ( 'NONE', #1358 ) ;
#11175 = CIRCLE ( 'NONE', #3940, 22.99899999999999878 ) ;
#11176 = AXIS2_PLACEMENT_3D ( 'NONE', #1682, #10987, #1627 ) ;
#11177 = EDGE_LOOP ( 'NONE', ( #11414, #11118, #841, #8386 ) ) ;
#11178 = CARTESIAN_POINT ( 'NONE',  ( 0.000000000000000000, 0.000000000000000000, 0.000000000000000000 ) ) ;
#11179 = CARTESIAN_POINT ( 'NONE',  ( 5.319643049700913728, -8.526005966359200272, 10.00000000000000000 ) ) ;
#11180 = DIRECTION ( 'NONE',  ( -1.000000000000000000, -0.000000000000000000, 0.000000000000000000 ) ) ;
#11181 = CARTESIAN_POINT ( 'NONE',  ( 0.000000000000000000, 0.000000000000000000, 0.000000000000000000 ) ) ;
#11182 = COLOUR_RGB ( '', 0.66274510, 0.83137255, 0.94901961) ;
#11183 = CARTESIAN_POINT ( 'NONE',  ( 4.071483724746831179, 10.33449570568845033, 3.747395293195558847E-16 ) ) ;
#11184 = CIRCLE ( 'NONE', #4708, 24.80000000000000071 ) ;
#11185 = DIRECTION ( 'NONE',  ( 0.000000000000000000, 0.000000000000000000, 1.000000000000000000 ) ) ;
#11186 = CARTESIAN_POINT ( 'NONE',  ( 0.000000000000000000, -20.93895013827591001, 13.28910708463121360 ) ) ;
#11187 = ADVANCED_FACE ( 'NONE', ( #2157 ), #10788, .T. ) ;
#11188 = EDGE_LOOP ( 'NONE', ( #3401, #5210, #2463, #562 ) ) ;
#11189 = ORIENTED_EDGE ( 'NONE', *, *, #8405, .F. ) ;
#11190 = CIRCLE ( 'NONE', #2782, 9.599999999999997868 ) ;
#11191 = VERTEX_POINT ( 'NONE', #8023 ) ;
#11192 = DIRECTION ( 'NONE',  ( -1.000000000000000000, 0.000000000000000000, -0.000000000000000000 ) ) ;
#11193 = CARTESIAN_POINT ( 'NONE',  ( 3.000000000000000888, -24.75110766671651064, -1.556492618230893132 ) ) ;
#11194 = VECTOR ( 'NONE', #1320, 1000.000000000000000 ) ;
#11195 = CARTESIAN_POINT ( 'NONE',  ( 3.000000000000000888, 0.000000000000000000, 0.000000000000000000 ) ) ;
#11196 = DIRECTION ( 'NONE',  ( 0.000000000000000000, 0.000000000000000000, 1.000000000000000000 ) ) ;
#11197 = EDGE_CURVE ( 'NONE', #11333, #992, #5164, .T. ) ;
#11198 = CARTESIAN_POINT ( 'NONE',  ( 3.000000000000000888, 9.039786367038837867, 21.14796121233199599 ) ) ;
#11199 = CARTESIAN_POINT ( 'NONE',  ( -11.21689850597007343, 9.520844388990626683, 3.747395293195558847E-16 ) ) ;
#11200 = CARTESIAN_POINT ( 'NONE',  ( -6.661525743073264394, 1.789546221321740793, 6.857782953271941950E-17 ) ) ;
#11201 = DIRECTION ( 'NONE',  ( 0.000000000000000000, -0.3090169943749349057, -0.9510565162951577500 ) ) ;
#11202 = ORIENTED_EDGE ( 'NONE', *, *, #5991, .T. ) ;
#11203 = EDGE_LOOP ( 'NONE', ( #7313, #495, #702, #9228 ) ) ;
#11204 = COLOUR_RGB ( '', 0.40784314, 0.44705882, 0.49803922) ;
#11205 = DIRECTION ( 'NONE',  ( 1.000000000000000000, -0.000000000000000000, 0.000000000000000000 ) ) ;
#11206 = ORIENTED_EDGE ( 'NONE', *, *, #1579, .T. ) ;
#11207 = ORIENTED_EDGE ( 'NONE', *, *, #9082, .F. ) ;
#11208 = CARTESIAN_POINT ( 'NONE',  ( 3.678979105947490780, -2.215585777442456550, 10.00000000000000000 ) ) ;
#11209 = AXIS2_PLACEMENT_3D ( 'NONE', #6729, #5073, #8639 ) ;
#11210 = LINE ( 'NONE', #10403, #7148 ) ;
#11211 = ORIENTED_EDGE ( 'NONE', *, *, #5471, .T. ) ;
#11212 = VECTOR ( 'NONE', #6588, 1000.000000000000000 ) ;
#11213 = FACE_OUTER_BOUND ( 'NONE', #9714, .T. ) ;
#11214 = LINE ( 'NONE', #62, #7860 ) ;
#11215 = CARTESIAN_POINT ( 'NONE',  ( -2.061894914253513456, 6.087690860853038899, 10.00000000000000000 ) ) ;
#11216 = CARTESIAN_POINT ( 'NONE',  ( 3.000000000000000888, 9.667200211209818761, 20.86861857134737264 ) ) ;
#11217 = CARTESIAN_POINT ( 'NONE',  ( 3.000000000000000888, -20.41249101028205004, -9.589108953448107542 ) ) ;
#11218 = VERTEX_POINT ( 'NONE', #438 ) ;
#11219 = EDGE_LOOP ( 'NONE', ( #4477, #10672 ) ) ;
#11220 = FACE_OUTER_BOUND ( 'NONE', #11107, .T. ) ;
#11221 = ORIENTED_EDGE ( 'NONE', *, *, #11265, .T. ) ;
#11222 = CARTESIAN_POINT ( 'NONE',  ( 0.2599977045011495624, -15.80854529698373945, 10.00000000000000000 ) ) ;
#11223 = EDGE_CURVE ( 'NONE', #9571, #1959, #2428, .T. ) ;
#11224 = DIRECTION ( 'NONE',  ( 1.000000000000000000, -0.000000000000000000, -0.000000000000000000 ) ) ;
#11225 = SURFACE_SIDE_STYLE ('',( #6563 ) ) ;
#11226 = VECTOR ( 'NONE', #7696, 1000.000000000000000 ) ;
#11227 = CARTESIAN_POINT ( 'NONE',  ( 1.500000000000000444, 1.039229259764490321, 24.77821629063822328 ) ) ;
#11228 = DIRECTION ( 'NONE',  ( -1.000000000000000000, 0.000000000000000000, 0.000000000000000000 ) ) ;
#11229 = CARTESIAN_POINT ( 'NONE',  ( -10.85385039129053197, -12.37615246896657872, 10.00000000000000000 ) ) ;
#11230 = EDGE_CURVE ( 'NONE', #8970, #3076, #85, .T. ) ;
#11231 = CARTESIAN_POINT ( 'NONE',  ( 7.449730884303669143, -3.679036338562942543, 6.857782953271941950E-17 ) ) ;
#11232 = DIRECTION ( 'NONE',  ( -1.000000000000000000, 0.000000000000000000, 0.000000000000000000 ) ) ;
#11233 = EDGE_CURVE ( 'NONE', #3964, #11218, #2236, .T. ) ;
#11234 = DIRECTION ( 'NONE',  ( -1.000000000000000000, 0.000000000000000000, 0.000000000000000000 ) ) ;
#11235 = ORIENTED_EDGE ( 'NONE', *, *, #8174, .T. ) ;
#11236 = EDGE_CURVE ( 'NONE', #1419, #6719, #6151, .T. ) ;
#11237 = ORIENTED_EDGE ( 'NONE', *, *, #6325, .F. ) ;
#11238 = AXIS2_PLACEMENT_3D ( 'NONE', #5781, #9565, #9447 ) ;
#11239 = VERTEX_POINT ( 'NONE', #8715 ) ;
#11240 = DIRECTION ( 'NONE',  ( 0.000000000000000000, 0.5000000000000011102, -0.8660254037844381525 ) ) ;
#11241 = CARTESIAN_POINT ( 'NONE',  ( 10.51453309316909568, -0.3307463982597985686, 10.00000000000000000 ) ) ;
#11242 = CARTESIAN_POINT ( 'NONE',  ( 17.50000000000000000, 0.000000000000000000, 10.00000000000000000 ) ) ;
#11243 = CARTESIAN_POINT ( 'NONE',  ( -8.111627617515257072, 3.498804908652022316, 3.747395293195558847E-16 ) ) ;
#11244 = CARTESIAN_POINT ( 'NONE',  ( 1.499999999999999556, -1.039229259764661961, 24.77821629063821263 ) ) ;
#11245 = CARTESIAN_POINT ( 'NONE',  ( 3.000000000000000888, 0.000000000000000000, 0.000000000000000000 ) ) ;
#11246 = VERTEX_POINT ( 'NONE', #7908 ) ;
#11247 = ORIENTED_EDGE ( 'NONE', *, *, #5232, .F. ) ;
#11248 = ORIENTED_EDGE ( 'NONE', *, *, #3771, .T. ) ;
#11249 = VERTEX_POINT ( 'NONE', #10538 ) ;
#11250 = CARTESIAN_POINT ( 'NONE',  ( 0.000000000000000000, -19.74380051311532114, -11.79560690673893042 ) ) ;
#11251 = ADVANCED_FACE ( 'NONE', ( #7961 ), #6922, .T. ) ;
#11252 = CIRCLE ( 'NONE', #8519, 22.99899999999999523 ) ;
#11253 = DIRECTION ( 'NONE',  ( -1.000000000000000000, 0.000000000000000000, 0.000000000000000000 ) ) ;
#11254 = DIRECTION ( 'NONE',  ( 0.000000000000000000, 0.000000000000000000, 1.000000000000000000 ) ) ;
#11255 = CARTESIAN_POINT ( 'NONE',  ( 3.000000000000000888, 12.88318129270205148, -18.51065745848364230 ) ) ;
#11256 = EDGE_CURVE ( 'NONE', #5746, #10699, #3219, .T. ) ;
#11257 = CYLINDRICAL_SURFACE ( 'NONE', #9656, 1.500000000000000222 ) ;
#11258 = CARTESIAN_POINT ( 'NONE',  ( 16.46093749971205611, -1.349437486485979498, 3.747395293195558847E-16 ) ) ;
#11259 = CARTESIAN_POINT ( 'NONE',  ( 0.000000000000000000, 5.117118920208799437, -22.42251312757874260 ) ) ;
#11260 = DIRECTION ( 'NONE',  ( 0.000000000000000000, -0.9781476007338077983, 0.2079116908177493783 ) ) ;
#11261 = CARTESIAN_POINT ( 'NONE',  ( 3.000000000000000888, 0.000000000000000000, 0.000000000000000000 ) ) ;
#11262 = ORIENTED_EDGE ( 'NONE', *, *, #8539, .F. ) ;
#11263 = ORIENTED_EDGE ( 'NONE', *, *, #823, .T. ) ;
#11264 = LINE ( 'NONE', #2878, #795 ) ;
#11265 = EDGE_CURVE ( 'NONE', #9763, #5965, #557, .T. ) ;
#11266 = ORIENTED_EDGE ( 'NONE', *, *, #4192, .T. ) ;
#11267 = DIRECTION ( 'NONE',  ( -1.000000000000000000, 0.000000000000000000, -0.000000000000000000 ) ) ;
#11268 = DIRECTION ( 'NONE',  ( 0.000000000000000000, 0.7431448254773909134, 0.6691306063588619013 ) ) ;
#11269 = VECTOR ( 'NONE', #5633, 1000.000000000000000 ) ;
#11270 = ORIENTED_EDGE ( 'NONE', *, *, #7095, .F. ) ;
#11271 = CYLINDRICAL_SURFACE ( 'NONE', #8482, 9.599999999999997868 ) ;
#11272 = CARTESIAN_POINT ( 'NONE',  ( 16.50000000000000355, 0.000000000000000000, 10.00000000000000000 ) ) ;
#11273 = CARTESIAN_POINT ( 'NONE',  ( 0.2749788638910972693, -16.81181333738675221, 6.857782953271941950E-17 ) ) ;
#11274 = CARTESIAN_POINT ( 'NONE',  ( 3.000000000000000888, 5.117118920208799437, -22.42251312757874260 ) ) ;
#11275 = DIRECTION ( 'NONE',  ( -1.000000000000000000, -0.000000000000000000, 0.000000000000000000 ) ) ;
#11276 = CARTESIAN_POINT ( 'NONE',  ( 1.499999999999999556, -23.88662356770110762, -6.668524164681869593 ) ) ;
#11277 = ORIENTED_EDGE ( 'NONE', *, *, #8626, .T. ) ;
#11278 = AXIS2_PLACEMENT_3D ( 'NONE', #2080, #10520, #4217 ) ;
#11279 = EDGE_LOOP ( 'NONE', ( #11669, #6959, #6964, #9438 ) ) ;
#11280 = DIRECTION ( 'NONE',  ( 0.000000000000000000, -0.9135454576425964257, -0.4067366430758103668 ) ) ;
#11281 = ORIENTED_EDGE ( 'NONE', *, *, #1124, .T. ) ;
#11282 = CARTESIAN_POINT ( 'NONE',  ( -3.562082835880472587, -15.28349083755603743, 10.00000000000000000 ) ) ;
#11283 = DIRECTION ( 'NONE',  ( -1.000000000000000000, 0.000000000000000000, 0.000000000000000000 ) ) ;
#11284 =( NAMED_UNIT ( * ) PLANE_ANGLE_UNIT ( ) SI_UNIT ( $, .RADIAN. ) );
#11285 = CARTESIAN_POINT ( 'NONE',  ( 3.000000000000000888, 0.000000000000000000, 22.99899999999999878 ) ) ;
#11286 = DIRECTION ( 'NONE',  ( 0.000000000000000000, -0.9510565162951565288, 0.3090169943749382364 ) ) ;
#11287 = CARTESIAN_POINT ( 'NONE',  ( 0.5005346673319861495, 15.27733729710888255, 10.00000000000000000 ) ) ;
#11288 = CARTESIAN_POINT ( 'NONE',  ( 3.000000000000000888, 0.000000000000000000, 0.000000000000000000 ) ) ;
#11289 = DIRECTION ( 'NONE',  ( 0.000000000000000000, 0.000000000000000000, 1.000000000000000000 ) ) ;
#11290 = CARTESIAN_POINT ( 'NONE',  ( 3.000000000000000888, 0.000000000000000000, 0.000000000000000000 ) ) ;
#11291 = CARTESIAN_POINT ( 'NONE',  ( 3.000000000000000888, 0.000000000000000000, 0.000000000000000000 ) ) ;
#11292 = ORIENTED_EDGE ( 'NONE', *, *, #7990, .T. ) ;
#11293 = AXIS2_PLACEMENT_3D ( 'NONE', #9933, #4556, #3578 ) ;
#11294 = LINE ( 'NONE', #9393, #8201 ) ;
#11295 = CARTESIAN_POINT ( 'NONE',  ( -5.868204859621552139, -7.421994279450156107, 10.00000000000000000 ) ) ;
#11296 = EDGE_CURVE ( 'NONE', #1972, #2776, #9627, .T. ) ;
#11297 = DIRECTION ( 'NONE',  ( 0.000000000000000000, 0.000000000000000000, 1.000000000000000000 ) ) ;
#11298 = EDGE_CURVE ( 'NONE', #3516, #3003, #1847, .T. ) ;
#11299 = CARTESIAN_POINT ( 'NONE',  ( -10.00031051369627022, 6.213292778946845729, 3.747395293195558847E-16 ) ) ;
#11300 = AXIS2_PLACEMENT_3D ( 'NONE', #189, #10299, #3939 ) ;
#11301 = LINE ( 'NONE', #2918, #1979 ) ;
#11302 = ORIENTED_EDGE ( 'NONE', *, *, #7900, .F. ) ;
#11303 = ORIENTED_EDGE ( 'NONE', *, *, #3214, .F. ) ;
#11304 = ORIENTED_EDGE ( 'NONE', *, *, #7778, .T. ) ;
#11305 = EDGE_CURVE ( 'NONE', #7198, #1881, #9473, .T. ) ;
#11306 = CARTESIAN_POINT ( 'NONE',  ( 3.000000000000000888, -5.135568396240178579, 21.96011696265489377 ) ) ;
#11307 = FACE_BOUND ( 'NONE', #4209, .T. ) ;
#11308 = CIRCLE ( 'NONE', #6799, 22.99899999999999523 ) ;
#11309 = CYLINDRICAL_SURFACE ( 'NONE', #11524, 9.599999999999997868 ) ;
#11310 = CYLINDRICAL_SURFACE ( 'NONE', #11883, 9.599999999999997868 ) ;
#11311 = AXIS2_PLACEMENT_3D ( 'NONE', #9949, #8301, #4385 ) ;
#11312 = CARTESIAN_POINT ( 'NONE',  ( 22.00000000000000000, 2.694222958124176809E-15, 0.000000000000000000 ) ) ;
#11313 = CARTESIAN_POINT ( 'NONE',  ( -3.562082835880472587, -15.28349083755603388, 3.747395293195558847E-16 ) ) ;
#11314 = CARTESIAN_POINT ( 'NONE',  ( 3.000000000000000888, 23.88662356770115736, 6.668524164681708832 ) ) ;
#11315 = EDGE_LOOP ( 'NONE', ( #458, #7702, #7705, #5890 ) ) ;
#11316 = ORIENTED_EDGE ( 'NONE', *, *, #9569, .T. ) ;
#11317 = AXIS2_PLACEMENT_3D ( 'NONE', #8041, #7291, #5465 ) ;
#11318 = DIRECTION ( 'NONE',  ( 0.000000000000000000, -0.1045284632676401482, -0.9945218953682748442 ) ) ;
#11319 = VERTEX_POINT ( 'NONE', #2277 ) ;
#11320 = EDGE_CURVE ( 'NONE', #9990, #7212, #4585, .T. ) ;
#11321 = DIRECTION ( 'NONE',  ( 0.000000000000000000, 0.000000000000000000, 1.000000000000000000 ) ) ;
#11322 = FACE_OUTER_BOUND ( 'NONE', #7179, .T. ) ;
#11323 = VERTEX_POINT ( 'NONE', #11639 ) ;
#11324 = CIRCLE ( 'NONE', #6043, 24.80000000000000071 ) ;
#11325 = CYLINDRICAL_SURFACE ( 'NONE', #11400, 20.00000000000000000 ) ;
#11326 = FACE_OUTER_BOUND ( 'NONE', #12064, .T. ) ;
#11327 = CARTESIAN_POINT ( 'NONE',  ( 8.547432504762587868, 12.33942397201039753, 6.857782953271941950E-17 ) ) ;
#11328 = DIRECTION ( 'NONE',  ( 0.000000000000000000, -0.3090169943749545012, 0.9510565162951513107 ) ) ;
#11329 = DIRECTION ( 'NONE',  ( -1.000000000000000000, -0.000000000000000000, -0.000000000000000000 ) ) ;
#11330 = ORIENTED_EDGE ( 'NONE', *, *, #3182, .F. ) ;
#11331 = ORIENTED_EDGE ( 'NONE', *, *, #11699, .T. ) ;
#11332 = CARTESIAN_POINT ( 'NONE',  ( 3.000000000000000888, 13.62355943574044481, -17.97274125076060258 ) ) ;
#11333 = VERTEX_POINT ( 'NONE', #3257 ) ;
#11334 = EDGE_CURVE ( 'NONE', #9734, #35, #6976, .T. ) ;
#11335 = CARTESIAN_POINT ( 'NONE',  ( 7.019749797092301513, 12.16723183298456057, 10.00000000000000000 ) ) ;
#11336 = CIRCLE ( 'NONE', #4110, 9.599999999999997868 ) ;
#11337 = DIRECTION ( 'NONE',  ( 0.000000000000000000, -0.3090169943749543902, 0.9510565162951514218 ) ) ;
#11338 = ORIENTED_EDGE ( 'NONE', *, *, #8268, .T. ) ;
#11339 = CARTESIAN_POINT ( 'NONE',  ( 0.000000000000000000, -19.10918332567947076, -15.80756504416710229 ) ) ;
#11340 = EDGE_CURVE ( 'NONE', #10253, #11877, #4198, .T. ) ;
#11341 = DIRECTION ( 'NONE',  ( -1.000000000000000000, 0.000000000000000000, 0.000000000000000000 ) ) ;
#11342 = CARTESIAN_POINT ( 'NONE',  ( 10.90031251054716499, 4.301772984117411269, 10.00000000000000000 ) ) ;
#11343 = CIRCLE ( 'NONE', #6064, 9.599999999999996092 ) ;
#11344 = DIRECTION ( 'NONE',  ( 0.000000000000000000, 0.000000000000000000, 1.000000000000000000 ) ) ;
#11345 = DIRECTION ( 'NONE',  ( -1.000000000000000000, -0.000000000000000000, -0.000000000000000000 ) ) ;
#11346 = CARTESIAN_POINT ( 'NONE',  ( 3.000000000000000000, 0.000000000000000000, 0.000000000000000000 ) ) ;
#11347 = ORIENTED_EDGE ( 'NONE', *, *, #5397, .T. ) ;
#11348 = CARTESIAN_POINT ( 'NONE',  ( -4.500000000000000888, -0.5000000000000000000, 3.000000000000000000 ) ) ;
#11349 = ORIENTED_EDGE ( 'NONE', *, *, #10200, .F. ) ;
#11350 = AXIS2_PLACEMENT_3D ( 'NONE', #6514, #9329, #11171 ) ;
#11351 = DIRECTION ( 'NONE',  ( 1.000000000000000000, 0.000000000000000000, -0.000000000000000000 ) ) ;
#11352 = CIRCLE ( 'NONE', #3537, 9.599999999999996092 ) ;
#11353 = CARTESIAN_POINT ( 'NONE',  ( -5.359287035704432434, 6.724520318541068242, 10.00000000000000000 ) ) ;
#11354 = CIRCLE ( 'NONE', #8029, 9.599999999999996092 ) ;
#11355 = DIRECTION ( 'NONE',  ( -1.000000000000000000, 0.000000000000000000, -0.000000000000000000 ) ) ;
#11356 = CARTESIAN_POINT ( 'NONE',  ( 5.835571643920557605, -9.386589068694828342, 10.00000000000000000 ) ) ;
#11357 = CARTESIAN_POINT ( 'NONE',  ( 10.35108484788238670, -9.702746953904560101, 6.857782953271941950E-17 ) ) ;
#11358 = CIRCLE ( 'NONE', #3153, 24.80000000000000071 ) ;
#11359 = CYLINDRICAL_SURFACE ( 'NONE', #5307, 9.599999999999997868 ) ;
#11360 = CIRCLE ( 'NONE', #8036, 3.000000000000000000 ) ;
#11361 = EDGE_LOOP ( 'NONE', ( #11211, #1405, #6709, #4683 ) ) ;
#11362 = CIRCLE ( 'NONE', #9405, 1.500000000000000222 ) ;
#11363 = EDGE_CURVE ( 'NONE', #730, #3959, #6722, .T. ) ;
#11364 = VERTEX_POINT ( 'NONE', #1607 ) ;
#11365 = DIRECTION ( 'NONE',  ( -1.000000000000000000, 0.000000000000000000, -0.000000000000000000 ) ) ;
#11366 = DIRECTION ( 'NONE',  ( -1.000000000000000000, 0.000000000000000000, 0.000000000000000000 ) ) ;
#11367 = CLOSED_SHELL ( 'NONE', ( #8910, #7126, #6808, #10039, #2773, #647, #8393, #2102, #6054 ) ) ;
#11368 = VERTEX_POINT ( 'NONE', #9008 ) ;
#11369 = EDGE_CURVE ( 'NONE', #9620, #8125, #873, .T. ) ;
#11370 = DIRECTION ( 'NONE',  ( -1.000000000000000000, 0.000000000000000000, 0.000000000000000000 ) ) ;
#11371 = DIRECTION ( 'NONE',  ( 1.000000000000000000, 0.000000000000000000, 0.000000000000000000 ) ) ;
#11372 = VECTOR ( 'NONE', #3612, 1000.000000000000000 ) ;
#11373 = DIRECTION ( 'NONE',  ( -1.000000000000000000, -0.000000000000000000, -0.000000000000000000 ) ) ;
#11374 = CARTESIAN_POINT ( 'NONE',  ( 7.019749797092834420, 12.16723183298349120, 3.747395293195558847E-16 ) ) ;
#11375 = EDGE_CURVE ( 'NONE', #6837, #679, #10100, .T. ) ;
#11376 = EDGE_CURVE ( 'NONE', #11900, #5379, #8504, .T. ) ;
#11377 = VECTOR ( 'NONE', #440, 1000.000000000000000 ) ;
#11378 = CARTESIAN_POINT ( 'NONE',  ( 3.000000000000000888, -7.432877647175354596, 21.76479567747239230 ) ) ;
#11379 = VERTEX_POINT ( 'NONE', #4416 ) ;
#11380 = CIRCLE ( 'NONE', #6102, 24.80000000000000071 ) ;
#11381 = EDGE_LOOP ( 'NONE', ( #7267, #869, #1893, #6601 ) ) ;
#11382 = EDGE_CURVE ( 'NONE', #8357, #4987, #3998, .T. ) ;
#11383 = CARTESIAN_POINT ( 'NONE',  ( 8.281812197879521165, -14.90260015151097228, 10.00000000000000000 ) ) ;
#11384 = ORIENTED_EDGE ( 'NONE', *, *, #1451, .T. ) ;
#11385 = CARTESIAN_POINT ( 'NONE',  ( 0.000000000000000000, 0.000000000000000000, 0.000000000000000000 ) ) ;
#11386 = DIRECTION ( 'NONE',  ( 0.000000000000000000, 0.000000000000000000, 1.000000000000000000 ) ) ;
#11387 = DIRECTION ( 'NONE',  ( 0.000000000000000000, 0.000000000000000000, 1.000000000000000000 ) ) ;
#11388 = ORIENTED_EDGE ( 'NONE', *, *, #11629, .T. ) ;
#11389 = AXIS2_PLACEMENT_3D ( 'NONE', #12089, #8365, #5609 ) ;
#11390 = CARTESIAN_POINT ( 'NONE',  ( 0.000000000000000000, 9.589108953447894379, 20.41249101028215307 ) ) ;
#11391 = DIRECTION ( 'NONE',  ( 0.000000000000000000, -0.9945218953682721796, -0.1045284632676635878 ) ) ;
#11392 = CARTESIAN_POINT ( 'NONE',  ( 7.619603487155711008, -11.82824555707797387, 6.857782953271941950E-17 ) ) ;
#11393 = DIRECTION ( 'NONE',  ( 1.000000000000000000, 0.000000000000000000, 0.000000000000000000 ) ) ;
#11394 = ORIENTED_EDGE ( 'NONE', *, *, #10698, .T. ) ;
#11395 = DIRECTION ( 'NONE',  ( -1.000000000000000000, -0.000000000000000000, 0.000000000000000000 ) ) ;
#11396 = ORIENTED_EDGE ( 'NONE', *, *, #1432, .T. ) ;
#11397 = ORIENTED_EDGE ( 'NONE', *, *, #4942, .F. ) ;
#11398 = CARTESIAN_POINT ( 'NONE',  ( 1.500000000000000444, -15.40502424595132247, -19.43515443678418464 ) ) ;
#11399 = ORIENTED_EDGE ( 'NONE', *, *, #4639, .F. ) ;
#11400 = AXIS2_PLACEMENT_3D ( 'NONE', #5519, #11145, #5703 ) ;
#11401 = CARTESIAN_POINT ( 'NONE',  ( 12.96212312671954514, -3.473279994529783199, 10.00000000000000000 ) ) ;
#11402 = CARTESIAN_POINT ( 'NONE',  ( 3.000000000000000888, 22.21333432029563681, 11.02759168516752730 ) ) ;
#11403 = ORIENTED_EDGE ( 'NONE', *, *, #11773, .T. ) ;
#11404 = FACE_OUTER_BOUND ( 'NONE', #2819, .T. ) ;
#11405 = CARTESIAN_POINT ( 'NONE',  ( 3.000000000000000888, 24.45282072769600745, 4.135161237383664812 ) ) ;
#11406 = CARTESIAN_POINT ( 'NONE',  ( 5.343773788080183884, 10.82393792025544421, 10.00000000000000000 ) ) ;
#11407 = EDGE_CURVE ( 'NONE', #1145, #8746, #5373, .T. ) ;
#11408 = AXIS2_PLACEMENT_3D ( 'NONE', #5752, #10143, #4645 ) ;
#11409 = CARTESIAN_POINT ( 'NONE',  ( 3.000000000000000888, -16.85990652506910692, 15.64281154287591669 ) ) ;
#11410 = CARTESIAN_POINT ( 'NONE',  ( 0.2599977045009999599, -15.80854529698373589, 3.747395293195558847E-16 ) ) ;
#11411 = DIRECTION ( 'NONE',  ( 0.000000000000000000, 0.9510565162951521989, 0.3090169943749515036 ) ) ;
#11412 = ORIENTED_EDGE ( 'NONE', *, *, #11783, .T. ) ;
#11413 = DIRECTION ( 'NONE',  ( 1.000000000000000000, 0.000000000000000000, 0.000000000000000000 ) ) ;
#11414 = ORIENTED_EDGE ( 'NONE', *, *, #1195, .T. ) ;
#11415 = EDGE_CURVE ( 'NONE', #8186, #4467, #7716, .T. ) ;
#11416 = ORIENTED_EDGE ( 'NONE', *, *, #2052, .T. ) ;
#11417 = CIRCLE ( 'NONE', #10830, 3.500000000000000000 ) ;
#11418 = DIRECTION ( 'NONE',  ( 0.000000000000000000, 0.4999999999999948375, 0.8660254037844415942 ) ) ;
#11419 = CARTESIAN_POINT ( 'NONE',  ( 7.357672848543034050, 2.125097602832379806, 10.00000000000000000 ) ) ;
#11420 = CARTESIAN_POINT ( 'NONE',  ( 1.500000000000000444, 23.24434456306325103, 8.645255683529084578 ) ) ;
#11421 = CARTESIAN_POINT ( 'NONE',  ( -9.386162357322616501, -4.067606288967439809, 10.00000000000000000 ) ) ;
#11422 = CARTESIAN_POINT ( 'NONE',  ( -10.11701526667143725, 11.92482893257633414, 6.857782953271941950E-17 ) ) ;
#11423 = VECTOR ( 'NONE', #8659, 1000.000000000000000 ) ;
#11424 = DIRECTION ( 'NONE',  ( 0.000000000000000000, 0.000000000000000000, 1.000000000000000000 ) ) ;
#11425 = ORIENTED_EDGE ( 'NONE', *, *, #6455, .F. ) ;
#11426 = EDGE_LOOP ( 'NONE', ( #9133, #11025, #7360, #291 ) ) ;
#11427 = CARTESIAN_POINT ( 'NONE',  ( -10.00000000000000000, 0.000000000000000000, 0.000000000000000000 ) ) ;
#11428 = DIRECTION ( 'NONE',  ( 0.000000000000000000, 0.000000000000000000, 1.000000000000000000 ) ) ;
#11429 = AXIS2_PLACEMENT_3D ( 'NONE', #7278, #3623, #9921 ) ;
#11430 = LINE ( 'NONE', #6770, #7586 ) ;
#11431 = DIRECTION ( 'NONE',  ( 1.000000000000000000, -0.000000000000000000, 0.000000000000000000 ) ) ;
#11432 = CARTESIAN_POINT ( 'NONE',  ( 3.000000000000000888, 7.402892494506579268, -21.30300407174355115 ) ) ;
#11433 = CARTESIAN_POINT ( 'NONE',  ( -3.141381368648054284, 10.98006565327106188, 3.747395293195558847E-16 ) ) ;
#11434 = CARTESIAN_POINT ( 'NONE',  ( 0.000000000000000000, 19.43515443678402832, 15.40502424595151609 ) ) ;
#11435 = EDGE_CURVE ( 'NONE', #6456, #8246, #5569, .T. ) ;
#11436 = ORIENTED_EDGE ( 'NONE', *, *, #3662, .F. ) ;
#11437 = ORIENTED_EDGE ( 'NONE', *, *, #8843, .F. ) ;
#11438 = CARTESIAN_POINT ( 'NONE',  ( 3.000000000000000888, -11.48910920600668462, -21.97817939804051335 ) ) ;
#11439 = ORIENTED_EDGE ( 'NONE', *, *, #9652, .T. ) ;
#11440 = CARTESIAN_POINT ( 'NONE',  ( 3.000000000000000888, 19.43515443678423793, -15.40502424595125497 ) ) ;
#11441 = DIRECTION ( 'NONE',  ( 1.000000000000000000, 0.000000000000000000, 0.000000000000000000 ) ) ;
#11442 = EDGE_CURVE ( 'NONE', #2229, #5263, #6733, .T. ) ;
#11443 = DIRECTION ( 'NONE',  ( 0.000000000000000000, -0.8660254037844328234, -0.5000000000000101030 ) ) ;
#11444 = ORIENTED_EDGE ( 'NONE', *, *, #587, .F. ) ;
#11445 = ADVANCED_FACE ( 'NONE', ( #6435 ), #11873, .T. ) ;
#11446 = DIRECTION ( 'NONE',  ( -1.000000000000000000, 0.000000000000000000, 0.000000000000000000 ) ) ;
#11447 = AXIS2_PLACEMENT_3D ( 'NONE', #3399, #3155, #2471 ) ;
#11448 = EDGE_CURVE ( 'NONE', #8331, #8912, #8209, .T. ) ;
#11449 = CARTESIAN_POINT ( 'NONE',  ( 3.000000000000000888, -21.97817939804031440, -11.48910920600707186 ) ) ;
#11450 = CARTESIAN_POINT ( 'NONE',  ( 10.38524206949620243, 10.73010674553377264, 6.857782953271941950E-17 ) ) ;
#11451 = CARTESIAN_POINT ( 'NONE',  ( 3.000000000000000888, -22.56530478845651544, 4.445336973060782348 ) ) ;
#11452 = ORIENTED_EDGE ( 'NONE', *, *, #4977, .T. ) ;
#11453 = DIRECTION ( 'NONE',  ( 0.000000000000000000, 0.000000000000000000, 1.000000000000000000 ) ) ;
#11454 = ORIENTED_EDGE ( 'NONE', *, *, #1724, .T. ) ;
#11455 = DIRECTION ( 'NONE',  ( -1.000000000000000000, 0.000000000000000000, 0.000000000000000000 ) ) ;
#11456 = ORIENTED_EDGE ( 'NONE', *, *, #523, .T. ) ;
#11457 = CIRCLE ( 'NONE', #903, 24.80000000000000071 ) ;
#11458 = CARTESIAN_POINT ( 'NONE',  ( 9.683839015878914935, 10.01260560230626595, 10.00000000000000000 ) ) ;
#11459 = EDGE_CURVE ( 'NONE', #4610, #6260, #282, .T. ) ;
#11460 = CARTESIAN_POINT ( 'NONE',  ( 0.000000000000000000, -22.54798042742717357, -0.4575788569254196636 ) ) ;
#11461 =( NAMED_UNIT ( * ) SI_UNIT ( $, .STERADIAN. ) SOLID_ANGLE_UNIT ( ) );
#11462 = DIRECTION ( 'NONE',  ( -1.000000000000000000, 0.000000000000000000, -0.000000000000000000 ) ) ;
#11463 = CARTESIAN_POINT ( 'NONE',  ( 3.000000000000002665, 4.898587196589412829E-16, -4.000000000000000000 ) ) ;
#11464 = CARTESIAN_POINT ( 'NONE',  ( 7.525577113297165610, 13.03378399180780889, 10.00000000000000000 ) ) ;
#11465 = AXIS2_PLACEMENT_3D ( 'NONE', #171, #6549, #3859 ) ;
#11466 = CARTESIAN_POINT ( 'NONE',  ( -10.19073739998278505, -11.62312336453203443, 3.747395293195558847E-16 ) ) ;
#11467 = DIRECTION ( 'NONE',  ( 0.000000000000000000, 0.000000000000000000, -1.000000000000000000 ) ) ;
#11468 = ADVANCED_FACE ( 'NONE', ( #10848 ), #6323, .T. ) ;
#11469 = CARTESIAN_POINT ( 'NONE',  ( 0.000000000000000000, 0.000000000000000000, 0.000000000000000000 ) ) ;
#11470 = PRODUCT_DEFINITION_SHAPE ( 'NONE', 'NONE',  #10317 ) ;
#11471 = VERTEX_POINT ( 'NONE', #6377 ) ;
#11472 = ADVANCED_FACE ( 'NONE', ( #802 ), #5399, .T. ) ;
#11473 = DIRECTION ( 'NONE',  ( -1.000000000000000000, 0.000000000000000000, 0.000000000000000000 ) ) ;
#11474 = CARTESIAN_POINT ( 'NONE',  ( -5.704017324792772570, 1.489539271746576743, 10.00000000000000000 ) ) ;
#11475 = CYLINDRICAL_SURFACE ( 'NONE', #5426, 24.80000000000000071 ) ;
#11476 = EDGE_CURVE ( 'NONE', #10278, #1752, #11933, .T. ) ;
#11477 = CARTESIAN_POINT ( 'NONE',  ( 10.54603994011899459, 5.199563424939650957, 10.00000000000000000 ) ) ;
#11478 = CARTESIAN_POINT ( 'NONE',  ( -7.327987143158983585, -11.36402271042705614, 6.857782953271941950E-17 ) ) ;
#11479 = DIRECTION ( 'NONE',  ( 0.000000000000000000, 0.000000000000000000, 1.000000000000000000 ) ) ;
#11480 = EDGE_CURVE ( 'NONE', #7835, #6502, #10448, .T. ) ;
#11481 = CARTESIAN_POINT ( 'NONE',  ( 3.000000000000000888, 0.000000000000000000, 0.000000000000000000 ) ) ;
#11482 = ORIENTED_EDGE ( 'NONE', *, *, #10598, .T. ) ;
#11483 = ORIENTED_EDGE ( 'NONE', *, *, #11415, .T. ) ;
#11484 = CARTESIAN_POINT ( 'NONE',  ( 1.499999999999999556, -13.28910708463113544, -20.93895013827595619 ) ) ;
#11485 = CARTESIAN_POINT ( 'NONE',  ( 16.46093749971205966, -1.349437486485980386, 10.00000000000000000 ) ) ;
#11486 = CARTESIAN_POINT ( 'NONE',  ( 1.500000000000000444, -13.72351598154911478, 20.65684170206487025 ) ) ;
#11487 = CARTESIAN_POINT ( 'NONE',  ( 0.000000000000000000, 0.000000000000000000, 0.000000000000000000 ) ) ;
#11488 = CARTESIAN_POINT ( 'NONE',  ( 3.000000000000000888, 0.000000000000000000, 0.000000000000000000 ) ) ;
#11489 = AXIS2_PLACEMENT_3D ( 'NONE', #1420, #3255, #10787 ) ;
#11490 = CARTESIAN_POINT ( 'NONE',  ( -2.069312577552832266, -12.54440658741723880, 3.747395293195558847E-16 ) ) ;
#11491 = DIRECTION ( 'NONE',  ( -1.000000000000000000, 0.000000000000000000, 0.000000000000000000 ) ) ;
#11492 = ORIENTED_EDGE ( 'NONE', *, *, #6741, .T. ) ;
#11493 = EDGE_LOOP ( 'NONE', ( #1642, #6247, #22, #9636 ) ) ;
#11494 = PRODUCT_CONTEXT ( 'NONE', #6763, 'mechanical' ) ;
#11495 = FACE_OUTER_BOUND ( 'NONE', #11909, .T. ) ;
#11496 = ORIENTED_EDGE ( 'NONE', *, *, #8102, .F. ) ;
#11497 = CARTESIAN_POINT ( 'NONE',  ( 10.64229886435067662, -13.41933351754326154, 6.857782953271941950E-17 ) ) ;
#11498 = AXIS2_PLACEMENT_3D ( 'NONE', #6891, #10635, #9709 ) ;
#11499 = DIRECTION ( 'NONE',  ( -1.000000000000000000, -0.000000000000000000, 0.000000000000000000 ) ) ;
#11500 = CYLINDRICAL_SURFACE ( 'NONE', #9642, 22.00000000000000000 ) ;
#11501 = DIRECTION ( 'NONE',  ( -1.000000000000000000, 0.000000000000000000, 0.000000000000000000 ) ) ;
#11502 = EDGE_LOOP ( 'NONE', ( #8470, #7351, #3231, #6810 ) ) ;
#11503 = CARTESIAN_POINT ( 'NONE',  ( 3.000000000000000888, 22.42251312757879234, 5.117118920208566735 ) ) ;
#11504 = DIRECTION ( 'NONE',  ( -1.000000000000000000, -0.000000000000000000, -0.000000000000000000 ) ) ;
#11505 = CARTESIAN_POINT ( 'NONE',  ( 13.92981926110967450, -3.738495919395730116, 6.857782953271941950E-17 ) ) ;
#11506 = CIRCLE ( 'NONE', #10525, 18.49999999999999645 ) ;
#11507 = AXIS2_PLACEMENT_3D ( 'NONE', #5225, #10734, #8903 ) ;
#11508 = ORIENTED_EDGE ( 'NONE', *, *, #11846, .F. ) ;
#11509 = CARTESIAN_POINT ( 'NONE',  ( 3.000000000000000888, 0.000000000000000000, 0.000000000000000000 ) ) ;
#11510 = ORIENTED_EDGE ( 'NONE', *, *, #2578, .T. ) ;
#11511 = DIRECTION ( 'NONE',  ( 0.000000000000000000, 0.000000000000000000, 1.000000000000000000 ) ) ;
#11512 = EDGE_LOOP ( 'NONE', ( #10295, #11189, #11292, #1033 ) ) ;
#11513 = EDGE_CURVE ( 'NONE', #4392, #10744, #9283, .T. ) ;
#11514 = CARTESIAN_POINT ( 'NONE',  ( -7.594692469639083399, -9.901549393538205734, 10.00000000000000000 ) ) ;
#11515 = CIRCLE ( 'NONE', #1153, 24.80000000000000071 ) ;
#11516 = CARTESIAN_POINT ( 'NONE',  ( -7.228014483236704444E-17, 0.5000000000000005551, 3.000000000000000000 ) ) ;
#11517 = DIRECTION ( 'NONE',  ( -1.000000000000000000, -0.000000000000000000, 0.000000000000000000 ) ) ;
#11518 = CARTESIAN_POINT ( 'NONE',  ( -10.00000000000000000, 0.000000000000000000, 0.000000000000000000 ) ) ;
#11519 = CARTESIAN_POINT ( 'NONE',  ( -13.04979933117209967, -0.2127334381860513379, 10.00000000000000000 ) ) ;
#11520 = DIRECTION ( 'NONE',  ( -1.000000000000000000, -0.000000000000000000, 0.000000000000000000 ) ) ;
#11521 = CARTESIAN_POINT ( 'NONE',  ( 0.000000000000000000, -22.83456483164687256, -2.745295967526231173 ) ) ;
#11523 = EDGE_CURVE ( 'NONE', #9363, #1910, #6159, .T. ) ;
#11522 = CIRCLE ( 'NONE', #7203, 9.599999999999999645 ) ;
#11524 = AXIS2_PLACEMENT_3D ( 'NONE', #10387, #4822, #6826 ) ;
#11525 = DIRECTION ( 'NONE',  ( 1.000000000000000000, 0.000000000000000000, 0.000000000000000000 ) ) ;
#11526 = CARTESIAN_POINT ( 'NONE',  ( 3.000000000000000888, 12.88318129270205148, -18.51065745848364230 ) ) ;
#11527 = EDGE_CURVE ( 'NONE', #7105, #9539, #5175, .T. ) ;
#11528 = AXIS2_PLACEMENT_3D ( 'NONE', #10396, #3910, #5930 ) ;
#11529 = ORIENTED_EDGE ( 'NONE', *, *, #3559, .F. ) ;
#11530 = ORIENTED_EDGE ( 'NONE', *, *, #11840, .F. ) ;
#11531 = VERTEX_POINT ( 'NONE', #10286 ) ;
#11532 = DIRECTION ( 'NONE',  ( 0.000000000000000000, 0.000000000000000000, 1.000000000000000000 ) ) ;
#11533 = CARTESIAN_POINT ( 'NONE',  ( -6.012500708481080203, 0.06204199954272103523, 10.00000000000000000 ) ) ;
#11534 = VECTOR ( 'NONE', #5363, 1000.000000000000000 ) ;
#11535 = DIRECTION ( 'NONE',  ( -1.000000000000000000, -0.000000000000000000, 0.000000000000000000 ) ) ;
#11536 = VECTOR ( 'NONE', #7605, 1000.000000000000000 ) ;
#11537 = CARTESIAN_POINT ( 'NONE',  ( -6.506554845699742629, -8.196137552274390004, 10.00000000000000000 ) ) ;
#11538 = CARTESIAN_POINT ( 'NONE',  ( 13.99323099382916169, 4.495563823643927037, 6.857782953271941950E-17 ) ) ;
#11539 = DIRECTION ( 'NONE',  ( 0.000000000000000000, -0.5000000000000072164, 0.8660254037844344888 ) ) ;
#11540 = CARTESIAN_POINT ( 'NONE',  ( 3.000000000000000888, 0.000000000000000000, 0.000000000000000000 ) ) ;
#11541 = ORIENTED_EDGE ( 'NONE', *, *, #9829, .F. ) ;
#11542 = AXIS2_PLACEMENT_3D ( 'NONE', #2523, #8030, #11764 ) ;
#11543 = AXIS2_PLACEMENT_3D ( 'NONE', #12046, #7454, #6310 ) ;
#11544 = AXIS2_PLACEMENT_3D ( 'NONE', #5221, #8098, #689 ) ;
#11545 = VERTEX_POINT ( 'NONE', #3862 ) ;
#11546 = CARTESIAN_POINT ( 'NONE',  ( 3.000000000000000888, 17.35216073792464542, -17.71842311621511712 ) ) ;
#11547 = PRESENTATION_LAYER_ASSIGNMENT (  '', '', ( #799 ) ) ;
#11548 = CARTESIAN_POINT ( 'NONE',  ( 3.000000000000000888, 2.062268319295562424, 22.90635393027947231 ) ) ;
#11549 = PLANE ( 'NONE',  #11498 ) ;
#11550 = CYLINDRICAL_SURFACE ( 'NONE', #5835, 3.000000000000000000 ) ;
#11551 = AXIS2_PLACEMENT_3D ( 'NONE', #6406, #899, #3839 ) ;
#11552 = AXIS2_PLACEMENT_3D ( 'NONE', #6483, #7328, #5442 ) ;
#11553 = CARTESIAN_POINT ( 'NONE',  ( -8.457858257354885723, -3.686763380685289970, 3.747395293195558847E-16 ) ) ;
#11554 = EDGE_CURVE ( 'NONE', #5010, #8709, #3564, .T. ) ;
#11555 = CARTESIAN_POINT ( 'NONE',  ( 3.000000000000000888, 4.445336973061170482, -22.56530478845644794 ) ) ;
#11556 = VERTEX_POINT ( 'NONE', #9550 ) ;
#11557 = ORIENTED_EDGE ( 'NONE', *, *, #4970, .T. ) ;
#11558 = CARTESIAN_POINT ( 'NONE',  ( 0.000000000000000000, 0.000000000000000000, 0.000000000000000000 ) ) ;
#11559 = CARTESIAN_POINT ( 'NONE',  ( 10.38524206949726469, 10.73010674553377797, 10.00000000000000000 ) ) ;
#11560 = VECTOR ( 'NONE', #27, 1000.000000000000000 ) ;
#11561 = ORIENTED_EDGE ( 'NONE', *, *, #8542, .T. ) ;
#11562 = CIRCLE ( 'NONE', #5672, 9.599999999999999645 ) ;
#11563 = DIRECTION ( 'NONE',  ( -1.000000000000000000, 0.000000000000000000, -0.000000000000000000 ) ) ;
#11564 = CARTESIAN_POINT ( 'NONE',  ( 8.000000000000000000, 0.000000000000000000, 0.000000000000000000 ) ) ;
#11565 = ADVANCED_FACE ( 'NONE', ( #11326 ), #6669, .T. ) ;
#11566 = AXIS2_PLACEMENT_3D ( 'NONE', #3059, #3913, #2016 ) ;
#11567 = LINE ( 'NONE', #3295, #10083 ) ;
#11568 = EDGE_LOOP ( 'NONE', ( #8792, #10234, #11851, #5178 ) ) ;
#11569 = CARTESIAN_POINT ( 'NONE',  ( 0.000000000000000000, 0.000000000000000000, 0.000000000000000000 ) ) ;
#11570 = FACE_OUTER_BOUND ( 'NONE', #11177, .T. ) ;
#11571 = CARTESIAN_POINT ( 'NONE',  ( 9.056240860197961595, 7.682302481599242228, 6.857782953271941950E-17 ) ) ;
#11572 = AXIS2_PLACEMENT_3D ( 'NONE', #559, #7964, #5093 ) ;
#11573 = PRODUCT ( 'cap', 'cap', '', ( #11494 ) ) ;
#11574 = ORIENTED_EDGE ( 'NONE', *, *, #2115, .T. ) ;
#11575 = AXIS2_PLACEMENT_3D ( 'NONE', #8078, #10836, #9730 ) ;
#11576 = CARTESIAN_POINT ( 'NONE',  ( 3.000000000000000888, 9.039786367038837867, 21.14796121233199599 ) ) ;
#11577 = VERTEX_POINT ( 'NONE', #1106 ) ;
#11578 = DIRECTION ( 'NONE',  ( -1.000000000000000000, -0.000000000000000000, -0.000000000000000000 ) ) ;
#11579 = ORIENTED_EDGE ( 'NONE', *, *, #4443, .F. ) ;
#11580 = CARTESIAN_POINT ( 'NONE',  ( -3.937910939466569005, -8.732312745279401156, 10.00000000000000000 ) ) ;
#11581 = AXIS2_PLACEMENT_3D ( 'NONE', #2321, #10591, #9787 ) ;
#11582 = CARTESIAN_POINT ( 'NONE',  ( 3.000000000000000888, -5.117118920208326038, -22.42251312757885273 ) ) ;
#11583 =( NAMED_UNIT ( * ) PLANE_ANGLE_UNIT ( ) SI_UNIT ( $, .RADIAN. ) );
#11584 = AXIS2_PLACEMENT_3D ( 'NONE', #9470, #3719, #9408 ) ;
#11585 = CARTESIAN_POINT ( 'NONE',  ( 3.000000000000000888, -19.29833442572351743, -11.67026512804567062 ) ) ;
#11586 = DIRECTION ( 'NONE',  ( -1.000000000000000000, -0.000000000000000000, -0.000000000000000000 ) ) ;
#11587 = CARTESIAN_POINT ( 'NONE',  ( -12.72059027619867955, -3.407653011836159873, 10.00000000000000000 ) ) ;
#11588 = FACE_OUTER_BOUND ( 'NONE', #10318, .T. ) ;
#11589 = CARTESIAN_POINT ( 'NONE',  ( 3.000000000000000888, 0.000000000000000000, 0.000000000000000000 ) ) ;
#11590 = DIRECTION ( 'NONE',  ( -1.000000000000000000, 0.000000000000000000, 0.000000000000000000 ) ) ;
#11591 = DIRECTION ( 'NONE',  ( -1.000000000000000000, 0.000000000000000000, 0.000000000000000000 ) ) ;
#11592 = ORIENTED_EDGE ( 'NONE', *, *, #2881, .F. ) ;
#11593 = ADVANCED_FACE ( 'NONE', ( #3012 ), #8019, .F. ) ;
#11594 = STYLED_ITEM ( 'NONE', ( #3407 ), #4621 ) ;
#11595 = DIRECTION ( 'NONE',  ( 0.000000000000000000, 0.000000000000000000, -1.000000000000000000 ) ) ;
#11596 = EDGE_CURVE ( 'NONE', #7251, #2827, #6308, .T. ) ;
#11597 = CARTESIAN_POINT ( 'NONE',  ( 0.000000000000000000, -24.45282072769597903, -4.135161237383833566 ) ) ;
#11598 = ADVANCED_FACE ( 'NONE', ( #988 ), #4729, .T. ) ;
#11599 = CARTESIAN_POINT ( 'NONE',  ( -2.433178163897189883, 9.086443520544605690, 10.00000000000000000 ) ) ;
#11600 = VECTOR ( 'NONE', #8635, 1000.000000000000000 ) ;
#11601 = CARTESIAN_POINT ( 'NONE',  ( 1.124919223378051392, -13.78906249641291559, 6.857782953271941950E-17 ) ) ;
#11602 = CARTESIAN_POINT ( 'NONE',  ( 3.000000000000000888, -12.88318129270165890, -18.51065745848391586 ) ) ;
#11603 = DIRECTION ( 'NONE',  ( -1.000000000000000000, 0.000000000000000000, -0.000000000000000000 ) ) ;
#11604 = ORIENTED_EDGE ( 'NONE', *, *, #9499, .F. ) ;
#11605 = ORIENTED_EDGE ( 'NONE', *, *, #1882, .F. ) ;
#11606 = AXIS2_PLACEMENT_3D ( 'NONE', #7019, #606, #11677 ) ;
#11607 = VERTEX_POINT ( 'NONE', #2026 ) ;
#11608 = CARTESIAN_POINT ( 'NONE',  ( 3.000000000000000888, -14.74749645579999857, -17.06259499759959297 ) ) ;
#11609 = CARTESIAN_POINT ( 'NONE',  ( 0.000000000000000000, -5.117118920208326038, -22.42251312757885273 ) ) ;
#11610 = DIRECTION ( 'NONE',  ( 0.000000000000000000, 0.000000000000000000, 1.000000000000000000 ) ) ;
#11611 = CARTESIAN_POINT ( 'NONE',  ( -6.430932688512553064, -6.885836206077581068, 3.747395293195558847E-16 ) ) ;
#11612 = DIRECTION ( 'NONE',  ( 0.000000000000000000, 0.5877852522924690293, 0.8090169943749504489 ) ) ;
#11613 = ORIENTED_EDGE ( 'NONE', *, *, #5583, .T. ) ;
#11614 = ORIENTED_EDGE ( 'NONE', *, *, #7018, .F. ) ;
#11615 = EDGE_CURVE ( 'NONE', #8841, #1098, #9039, .T. ) ;
#11616 = CARTESIAN_POINT ( 'NONE',  ( 12.50121531544689013, -6.953993600215019555, 10.00000000000000000 ) ) ;
#11617 = ORIENTED_EDGE ( 'NONE', *, *, #481, .F. ) ;
#11618 = VECTOR ( 'NONE', #1980, 1000.000000000000000 ) ;
#11619 = CARTESIAN_POINT ( 'NONE',  ( 3.000000000000000888, 11.79560690673899970, -19.74380051311527495 ) ) ;
#11620 = FACE_OUTER_BOUND ( 'NONE', #6181, .T. ) ;
#11621 = EDGE_CURVE ( 'NONE', #7393, #962, #8466, .T. ) ;
#11622 = DIRECTION ( 'NONE',  ( -1.000000000000000000, 0.000000000000000000, -0.000000000000000000 ) ) ;
#11623 = ORIENTED_EDGE ( 'NONE', *, *, #9218, .T. ) ;
#11624 = LINE ( 'NONE', #9612, #1637 ) ;
#11625 = EDGE_CURVE ( 'NONE', #1851, #9423, #3743, .T. ) ;
#11626 = CARTESIAN_POINT ( 'NONE',  ( 3.000000000000000888, -24.77821629063822328, 1.039229259764401947 ) ) ;
#11627 = CARTESIAN_POINT ( 'NONE',  ( 0.7062845326066684581, -10.79445016380498501, 6.857782953271941950E-17 ) ) ;
#11628 = ORIENTED_EDGE ( 'NONE', *, *, #444, .F. ) ;
#11629 = EDGE_CURVE ( 'NONE', #10824, #6719, #11214, .T. ) ;
#11630 = CARTESIAN_POINT ( 'NONE',  ( 3.000000000000000888, 15.13242714128119459, 17.31945870441152380 ) ) ;
#11631 = CARTESIAN_POINT ( 'NONE',  ( 3.000000000000000888, -23.05871956130116374, -9.128825345753257992 ) ) ;
#11632 = VERTEX_POINT ( 'NONE', #5704 ) ;
#11633 = CARTESIAN_POINT ( 'NONE',  ( -11.98301361336074500, 0.7816210414391656647, 10.00000000000000000 ) ) ;
#11634 = ORIENTED_EDGE ( 'NONE', *, *, #6898, .T. ) ;
#11635 = DIRECTION ( 'NONE',  ( -1.000000000000000000, 0.000000000000000000, 0.000000000000000000 ) ) ;
#11636 = CIRCLE ( 'NONE', #7732, 24.80000000000000071 ) ;
#11637 = ORIENTED_EDGE ( 'NONE', *, *, #8931, .T. ) ;
#11638 = DIRECTION ( 'NONE',  ( -0.000000000000000000, -0.000000000000000000, -1.000000000000000000 ) ) ;
#11639 = CARTESIAN_POINT ( 'NONE',  ( 3.000000000000000888, -20.65684170206481696, -13.72351598154918406 ) ) ;
#11640 = CARTESIAN_POINT ( 'NONE',  ( -9.650762677556034674, -3.270672451565360461, 10.00000000000000000 ) ) ;
#11641 = CARTESIAN_POINT ( 'NONE',  ( 0.000000000000000000, -21.30300407174367905, 7.402892494506218668 ) ) ;
#11642 = CARTESIAN_POINT ( 'NONE',  ( -1.872083171988683015, 14.23747171912756038, 3.747395293195558847E-16 ) ) ;
#11643 = CARTESIAN_POINT ( 'NONE',  ( 3.000000000000000888, 20.41249101028211754, 9.589108953447965433 ) ) ;
#11644 = CIRCLE ( 'NONE', #4420, 9.599999999999997868 ) ;
#11645 = ORIENTED_EDGE ( 'NONE', *, *, #11320, .F. ) ;
#11646 = LINE ( 'NONE', #10795, #8015 ) ;
#11647 = ORIENTED_EDGE ( 'NONE', *, *, #1791, .F. ) ;
#11648 = DIRECTION ( 'NONE',  ( -1.000000000000000000, -0.000000000000000000, -0.000000000000000000 ) ) ;
#11649 = CARTESIAN_POINT ( 'NONE',  ( 0.000000000000000000, -24.77821629063822328, 1.039229259764401947 ) ) ;
#11650 = AXIS2_PLACEMENT_3D ( 'NONE', #3805, #7397, #3918 ) ;
#11651 = CYLINDRICAL_SURFACE ( 'NONE', #1399, 9.599999999999997868 ) ;
#11652 = FACE_OUTER_BOUND ( 'NONE', #2705, .T. ) ;
#11653 = CARTESIAN_POINT ( 'NONE',  ( 6.242895496889244278, -5.302832405932367266, 10.00000000000000000 ) ) ;
#11654 = CARTESIAN_POINT ( 'NONE',  ( -9.650762677556027569, -3.270672451565358685, 6.857782953271941950E-17 ) ) ;
#11655 = DIRECTION ( 'NONE',  ( -1.000000000000000000, 0.000000000000000000, 0.000000000000000000 ) ) ;
#11656 = ORIENTED_EDGE ( 'NONE', *, *, #2783, .F. ) ;
#11657 = ADVANCED_FACE ( 'NONE', ( #3679 ), #10465, .T. ) ;
#11658 = ORIENTED_EDGE ( 'NONE', *, *, #1579, .F. ) ;
#11659 = EDGE_CURVE ( 'NONE', #11531, #1833, #9817, .T. ) ;
#11660 = CARTESIAN_POINT ( 'NONE',  ( 0.2599977045011495624, -15.80854529698373945, 10.00000000000000000 ) ) ;
#11661 = EDGE_CURVE ( 'NONE', #8512, #8970, #6609, .T. ) ;
#11662 = DIRECTION ( 'NONE',  ( -1.000000000000000000, -0.000000000000000000, -0.000000000000000000 ) ) ;
#11663 = CARTESIAN_POINT ( 'NONE',  ( 3.000000000000000888, 24.53384959170462665, -3.623565124516855640 ) ) ;
#11664 = CARTESIAN_POINT ( 'NONE',  ( 9.701579622837702033, -3.641351606116561612, 3.747395293195558847E-16 ) ) ;
#11665 = DIRECTION ( 'NONE',  ( 1.000000000000000000, -0.000000000000000000, -0.000000000000000000 ) ) ;
#11666 = ADVANCED_FACE ( 'NONE', ( #1962 ), #9433, .T. ) ;
#11667 = DIRECTION ( 'NONE',  ( -1.000000000000000000, 0.000000000000000000, 0.000000000000000000 ) ) ;
#11668 = ORIENTED_EDGE ( 'NONE', *, *, #81, .T. ) ;
#11669 = ORIENTED_EDGE ( 'NONE', *, *, #8409, .F. ) ;
#11670 = CARTESIAN_POINT ( 'NONE',  ( -9.783806739528735363, -9.162509837619124298, 10.00000000000000000 ) ) ;
#11671 = ORIENTED_EDGE ( 'NONE', *, *, #11923, .T. ) ;
#11672 = CARTESIAN_POINT ( 'NONE',  ( 3.000000000000000888, 0.000000000000000000, 0.000000000000000000 ) ) ;
#11673 = CYLINDRICAL_SURFACE ( 'NONE', #2216, 22.00000000000000000 ) ;
#11674 = AXIS2_PLACEMENT_3D ( 'NONE', #7666, #3026, #9564 ) ;
#11675 = DIRECTION ( 'NONE',  ( -1.000000000000000000, 0.000000000000000000, 0.000000000000000000 ) ) ;
#11676 = VERTEX_POINT ( 'NONE', #5764 ) ;
#11677 = DIRECTION ( 'NONE',  ( 0.000000000000000000, 0.000000000000000000, -1.000000000000000000 ) ) ;
#11678 = EDGE_CURVE ( 'NONE', #5404, #7624, #2382, .T. ) ;
#11679 = CARTESIAN_POINT ( 'NONE',  ( 0.000000000000000000, 17.31945870441167301, -15.13242714128102406 ) ) ;
#11680 = CARTESIAN_POINT ( 'NONE',  ( -0.1504880127286837288, 9.287785325659760005, 6.857782953271941950E-17 ) ) ;
#11681 = ORIENTED_EDGE ( 'NONE', *, *, #6580, .T. ) ;
#11682 = EDGE_CURVE ( 'NONE', #7675, #9669, #9230, .T. ) ;
#11683 = DIRECTION ( 'NONE',  ( 0.000000000000000000, 0.000000000000000000, 1.000000000000000000 ) ) ;
#11684 = AXIS2_PLACEMENT_3D ( 'NONE', #4644, #9350, #11196 ) ;
#11685 = EDGE_CURVE ( 'NONE', #5818, #8458, #11768, .T. ) ;
#11686 = CARTESIAN_POINT ( 'NONE',  ( 3.000000000000000888, 21.97702544527767188, -6.779701584702504391 ) ) ;
#11687 = ORIENTED_EDGE ( 'NONE', *, *, #2766, .F. ) ;
#11688 = CARTESIAN_POINT ( 'NONE',  ( -4.054747718262374789, -11.96785467447666029, 10.00000000000000000 ) ) ;
#11689 = CARTESIAN_POINT ( 'NONE',  ( 0.000000000000000000, 0.000000000000000000, 22.99899999999999878 ) ) ;
#11690 = DIRECTION ( 'NONE',  ( 0.000000000000000000, 0.000000000000000000, -1.000000000000000000 ) ) ;
#11691 = ORIENTED_EDGE ( 'NONE', *, *, #442, .T. ) ;
#11692 = CIRCLE ( 'NONE', #2915, 9.599999999999997868 ) ;
#11693 = DIRECTION ( 'NONE',  ( 0.000000000000000000, -0.6691306063588494668, -0.7431448254774020157 ) ) ;
#11694 = AXIS2_PLACEMENT_3D ( 'NONE', #525, #11662, #10747 ) ;
#11695 = CARTESIAN_POINT ( 'NONE',  ( 3.000000000000000888, -21.58580335785672233, -6.532525787311189269 ) ) ;
#11696 = CARTESIAN_POINT ( 'NONE',  ( 3.534825977509327366, -7.171832907601992879, 10.00000000000000000 ) ) ;
#11697 = CARTESIAN_POINT ( 'NONE',  ( 3.000000000000000888, 0.000000000000000000, 0.000000000000000000 ) ) ;
#11698 = CARTESIAN_POINT ( 'NONE',  ( -12.04643853703213452, -0.2059847383342608973, 3.747395293195558847E-16 ) ) ;
#11699 = EDGE_CURVE ( 'NONE', #2021, #9956, #8880, .T. ) ;
#11700 = CARTESIAN_POINT ( 'NONE',  ( 0.000000000000000000, -13.28910708463142498, 20.93895013827577145 ) ) ;
#11701 = ORIENTED_EDGE ( 'NONE', *, *, #2125, .T. ) ;
#11702 = FACE_OUTER_BOUND ( 'NONE', #95, .T. ) ;
#11703 = ORIENTED_EDGE ( 'NONE', *, *, #10846, .T. ) ;
#11704 = VECTOR ( 'NONE', #1757, 1000.000000000000000 ) ;
#11705 = DIRECTION ( 'NONE',  ( 1.000000000000000000, 0.000000000000000000, 0.000000000000000000 ) ) ;
#11706 = ORIENTED_EDGE ( 'NONE', *, *, #5778, .T. ) ;
#11707 = EDGE_CURVE ( 'NONE', #2848, #6354, #8054, .T. ) ;
#11708 = DIRECTION ( 'NONE',  ( -1.000000000000000000, -0.000000000000000000, 0.000000000000000000 ) ) ;
#11709 = LINE ( 'NONE', #8042, #1444 ) ;
#11710 = CARTESIAN_POINT ( 'NONE',  ( 4.503282398431824873, -2.806195971666264111, 10.00000000000000000 ) ) ;
#11711 = AXIS2_PLACEMENT_3D ( 'NONE', #3292, #8929, #891 ) ;
#11712 = CARTESIAN_POINT ( 'NONE',  ( -2.433178163897522506, 9.086443520544598584, 6.857782953271941950E-17 ) ) ;
#11713 = FACE_OUTER_BOUND ( 'NONE', #4595, .T. ) ;
#11714 = AXIS2_PLACEMENT_3D ( 'NONE', #5754, #8565, #3973 ) ;
#11715 = DIRECTION ( 'NONE',  ( -0.000000000000000000, -0.000000000000000000, -1.000000000000000000 ) ) ;
#11716 = ORIENTED_EDGE ( 'NONE', *, *, #1950, .T. ) ;
#11717 = ORIENTED_EDGE ( 'NONE', *, *, #11817, .T. ) ;
#11718 = AXIS2_PLACEMENT_3D ( 'NONE', #1020, #8490, #87 ) ;
#11719 = ORIENTED_EDGE ( 'NONE', *, *, #7012, .T. ) ;
#11720 = CARTESIAN_POINT ( 'NONE',  ( 2.103398428914359908, -12.69820342197951035, 10.00000000000000000 ) ) ;
#11721 = AXIS2_PLACEMENT_3D ( 'NONE', #5099, #5963, #10489 ) ;
#11722 = DIRECTION ( 'NONE',  ( 0.000000000000000000, 0.000000000000000000, -1.000000000000000000 ) ) ;
#11723 = CARTESIAN_POINT ( 'NONE',  ( 7.536008357046521944, 0.2705779428718260160, 3.747395293195558847E-16 ) ) ;
#11724 = CIRCLE ( 'NONE', #9972, 24.80000000000000071 ) ;
#11725 = DIRECTION ( 'NONE',  ( -1.000000000000000000, -0.000000000000000000, -0.000000000000000000 ) ) ;
#11726 = EDGE_CURVE ( 'NONE', #11784, #2212, #8653, .T. ) ;
#11727 = CIRCLE ( 'NONE', #4504, 24.80000000000000071 ) ;
#11728 = DIRECTION ( 'NONE',  ( -1.000000000000000000, 0.000000000000000000, -0.000000000000000000 ) ) ;
#11729 = VERTEX_POINT ( 'NONE', #11679 ) ;
#11730 = ORIENTED_EDGE ( 'NONE', *, *, #8616, .T. ) ;
#11731 = COLOUR_RGB ( '', 0.40784314, 0.44705882, 0.49803922) ;
#11732 = CONTEXT_DEPENDENT_SHAPE_REPRESENTATION ( #737, #7550 ) ;
#11733 = CARTESIAN_POINT ( 'NONE',  ( -4.384918567263696332, -12.91535881965571342, 10.00000000000000000 ) ) ;
#11734 = EDGE_LOOP ( 'NONE', ( #5599, #8454, #1772, #1032 ) ) ;
#11735 = CARTESIAN_POINT ( 'NONE',  ( 0.000000000000000000, 0.000000000000000000, 0.000000000000000000 ) ) ;
#11736 = ADVANCED_FACE ( 'NONE', ( #1343 ), #6058, .T. ) ;
#11737 = FACE_OUTER_BOUND ( 'NONE', #10336, .T. ) ;
#11738 = DIRECTION ( 'NONE',  ( 0.000000000000000000, 0.000000000000000000, 1.000000000000000000 ) ) ;
#11739 = VECTOR ( 'NONE', #7281, 1000.000000000000000 ) ;
#11740 = CARTESIAN_POINT ( 'NONE',  ( 0.000000000000000000, 0.000000000000000000, -5.000000000000000000 ) ) ;
#11741 = EDGE_LOOP ( 'NONE', ( #4312, #1306, #11756, #3686 ) ) ;
#11742 = EDGE_CURVE ( 'NONE', #8458, #10699, #7022, .T. ) ;
#11743 = FACE_OUTER_BOUND ( 'NONE', #10320, .T. ) ;
#11744 = EDGE_CURVE ( 'NONE', #3286, #8186, #1466, .T. ) ;
#11745 = DIRECTION ( 'NONE',  ( 0.000000000000000000, 0.000000000000000000, 1.000000000000000000 ) ) ;
#11746 = CARTESIAN_POINT ( 'NONE',  ( 7.737545192982509867, 9.111483571581276308, 6.857782953271941950E-17 ) ) ;
#11747 = EDGE_CURVE ( 'NONE', #4581, #9467, #8464, .T. ) ;
#11748 = DIRECTION ( 'NONE',  ( -1.000000000000000000, 0.000000000000000000, -0.000000000000000000 ) ) ;
#11749 = CARTESIAN_POINT ( 'NONE',  ( -10.00000000000000000, 0.000000000000000000, 0.000000000000000000 ) ) ;
#11750 = VECTOR ( 'NONE', #8853, 1000.000000000000000 ) ;
#11751 = ORIENTED_EDGE ( 'NONE', *, *, #1873, .T. ) ;
#11752 = AXIS2_PLACEMENT_3D ( 'NONE', #9848, #1699, #7192 ) ;
#11753 = CARTESIAN_POINT ( 'NONE',  ( 10.41236255589547177, -1.188820951657899361, 10.00000000000000000 ) ) ;
#11754 = DIRECTION ( 'NONE',  ( -1.000000000000000000, -0.000000000000000000, 0.000000000000000000 ) ) ;
#11755 = DIRECTION ( 'NONE',  ( 0.000000000000000000, 0.000000000000000000, 1.000000000000000000 ) ) ;
#11756 = ORIENTED_EDGE ( 'NONE', *, *, #5471, .F. ) ;
#11757 = CIRCLE ( 'NONE', #3757, 22.00000000000000000 ) ;
#11758 = CARTESIAN_POINT ( 'NONE',  ( 0.000000000000000000, 23.24434456306324748, 8.645255683529086355 ) ) ;
#11759 = CIRCLE ( 'NONE', #2777, 9.599999999999996092 ) ;
#11760 = DIRECTION ( 'NONE',  ( 0.000000000000000000, -0.2079116908177664480, 0.9781476007338040235 ) ) ;
#11761 = CARTESIAN_POINT ( 'NONE',  ( -9.023584016175229650, 3.917288190900558131, 10.00000000000000000 ) ) ;
#11762 = DIRECTION ( 'NONE',  ( 1.000000000000000000, 0.000000000000000000, 0.000000000000000000 ) ) ;
#11763 = CARTESIAN_POINT ( 'NONE',  ( 7.019749797092834420, 12.16723183298349120, 3.747395293195558847E-16 ) ) ;
#11764 = DIRECTION ( 'NONE',  ( 0.000000000000000000, -0.5877852522924631451, -0.8090169943749546677 ) ) ;
#11765 = CARTESIAN_POINT ( 'NONE',  ( 3.000000000000000888, 0.000000000000000000, 0.000000000000000000 ) ) ;
#11766 = CIRCLE ( 'NONE', #5913, 3.000000000000000000 ) ;
#11767 = VERTEX_POINT ( 'NONE', #7714 ) ;
#11768 = CIRCLE ( 'NONE', #6491, 22.99900000000000233 ) ;
#11769 = CARTESIAN_POINT ( 'NONE',  ( 0.000000000000000000, -15.13242714128131361, 17.31945870441142077 ) ) ;
#11770 = AXIS2_PLACEMENT_3D ( 'NONE', #5801, #9527, #10632 ) ;
#11771 = CARTESIAN_POINT ( 'NONE',  ( -10.00000000000000000, 0.000000000000000000, 0.000000000000000000 ) ) ;
#11772 = ORIENTED_EDGE ( 'NONE', *, *, #2920, .T. ) ;
#11773 = EDGE_CURVE ( 'NONE', #7424, #2472, #10989, .T. ) ;
#11774 = DIRECTION ( 'NONE',  ( 0.000000000000000000, 0.4999999999999948375, 0.8660254037844415942 ) ) ;
#11775 = DIRECTION ( 'NONE',  ( -1.000000000000000000, 0.000000000000000000, 0.000000000000000000 ) ) ;
#11776 = CARTESIAN_POINT ( 'NONE',  ( 6.689389171169565884, -4.795626085247176817, 10.00000000000000000 ) ) ;
#11777 = AXIS2_PLACEMENT_3D ( 'NONE', #8194, #7320, #11070 ) ;
#11778 = CARTESIAN_POINT ( 'NONE',  ( 9.246005348854470896, -6.405614325511344909, 6.857782953271941950E-17 ) ) ;
#11779 = SURFACE_STYLE_USAGE ( .BOTH. , #8045 ) ;
#11780 = CARTESIAN_POINT ( 'NONE',  ( 3.000000000000000888, 18.40266524480607657, -13.79477846460777357 ) ) ;
#11781 = VECTOR ( 'NONE', #6628, 1000.000000000000000 ) ;
#11782 = ORIENTED_EDGE ( 'NONE', *, *, #3978, .T. ) ;
#11783 = EDGE_CURVE ( 'NONE', #11174, #5068, #5329, .T. ) ;
#11784 = VERTEX_POINT ( 'NONE', #4967 ) ;
#11785 = ORIENTED_EDGE ( 'NONE', *, *, #6875, .T. ) ;
#11786 = CIRCLE ( 'NONE', #1427, 19.99999999999999645 ) ;
#11787 = CARTESIAN_POINT ( 'NONE',  ( 4.163410377374356486, -12.26152398776834396, 10.00000000000000000 ) ) ;
#11788 = DIRECTION ( 'NONE',  ( 0.000000000000000000, 0.000000000000000000, 1.000000000000000000 ) ) ;
#11789 = LINE ( 'NONE', #654, #8769 ) ;
#11790 = CARTESIAN_POINT ( 'NONE',  ( 0.5199114366211738947, 8.229807867079655281, 3.747395293195558847E-16 ) ) ;
#11791 = AXIS2_PLACEMENT_3D ( 'NONE', #2744, #7570, #5565 ) ;
#11792 = CARTESIAN_POINT ( 'NONE',  ( 3.000000000000000888, -11.48910920600699193, 21.97817939804035348 ) ) ;
#11793 = CARTESIAN_POINT ( 'NONE',  ( 0.000000000000000000, 24.53384959170462665, -3.623565124516855640 ) ) ;
#11794 = VERTEX_POINT ( 'NONE', #11449 ) ;
#11795 = ORIENTED_EDGE ( 'NONE', *, *, #7356, .F. ) ;
#11796 = ORIENTED_EDGE ( 'NONE', *, *, #4424, .T. ) ;
#11797 = DIRECTION ( 'NONE',  ( 0.000000000000000000, 0.1045284632676536929, -0.9945218953682732899 ) ) ;
#11798 = LINE ( 'NONE', #831, #2332 ) ;
#11799 = CARTESIAN_POINT ( 'NONE',  ( 0.000000000000000000, -13.79477846460808799, 18.40266524480583854 ) ) ;
#11800 = AXIS2_PLACEMENT_3D ( 'NONE', #269, #4807, #6696 ) ;
#11801 = DIRECTION ( 'NONE',  ( -1.000000000000000000, 0.000000000000000000, 0.000000000000000000 ) ) ;
#11802 = VERTEX_POINT ( 'NONE', #11626 ) ;
#11803 = CARTESIAN_POINT ( 'NONE',  ( 0.000000000000000000, 11.79560690673872436, 19.74380051311544193 ) ) ;
#11804 = DIRECTION ( 'NONE',  ( 0.000000000000000000, 0.8660254037844363761, 0.5000000000000039968 ) ) ;
#11805 = CARTESIAN_POINT ( 'NONE',  ( -9.960937504979705537, 0.8181230654449899165, 6.857782953271941950E-17 ) ) ;
#11806 = DIRECTION ( 'NONE',  ( 0.000000000000000000, 0.000000000000000000, 1.000000000000000000 ) ) ;
#11807 = DIRECTION ( 'NONE',  ( 0.000000000000000000, 0.8660254037844397068, -0.4999999999999980016 ) ) ;
#11808 = VERTEX_POINT ( 'NONE', #5022 ) ;
#11809 = EDGE_CURVE ( 'NONE', #1972, #1329, #4344, .T. ) ;
#11810 = ORIENTED_EDGE ( 'NONE', *, *, #3694, .F. ) ;
#11811 = CARTESIAN_POINT ( 'NONE',  ( 4.623190192904714557, -5.402202315098911356, 10.00000000000000000 ) ) ;
#11812 = EDGE_CURVE ( 'NONE', #4077, #384, #5999, .T. ) ;
#11813 = ORIENTED_EDGE ( 'NONE', *, *, #11985, .F. ) ;
#11814 = DIRECTION ( 'NONE',  ( -1.000000000000000000, -0.000000000000000000, 0.000000000000000000 ) ) ;
#11815 = EDGE_CURVE ( 'NONE', #4516, #7393, #425, .T. ) ;
#11816 = ORIENTED_EDGE ( 'NONE', *, *, #2058, .F. ) ;
#11817 = EDGE_CURVE ( 'NONE', #429, #9019, #828, .T. ) ;
#11818 = CARTESIAN_POINT ( 'NONE',  ( 3.000000000000000888, -6.779701584702886308, 21.97702544527755109 ) ) ;
#11819 = DIRECTION ( 'NONE',  ( 0.000000000000000000, 0.9945218953682736229, -0.1045284632676503622 ) ) ;
#11820 = CARTESIAN_POINT ( 'NONE',  ( 2.084091085258986897, 8.931495281877387171, 10.00000000000000000 ) ) ;
#11821 = DIRECTION ( 'NONE',  ( -1.000000000000000000, -0.000000000000000000, 0.000000000000000000 ) ) ;
#11822 = CARTESIAN_POINT ( 'NONE',  ( 7.983652613117083519, -10.39416588708253819, 3.747395293195558847E-16 ) ) ;
#11823 = FACE_OUTER_BOUND ( 'NONE', #8441, .T. ) ;
#11824 = ORIENTED_EDGE ( 'NONE', *, *, #11157, .F. ) ;
#11825 = DIRECTION ( 'NONE',  ( 0.000000000000000000, 0.000000000000000000, 1.000000000000000000 ) ) ;
#11826 = ORIENTED_EDGE ( 'NONE', *, *, #5702, .F. ) ;
#11827 = ADVANCED_FACE ( 'NONE', ( #11570 ), #3190, .T. ) ;
#11828 = CARTESIAN_POINT ( 'NONE',  ( 3.006682760306612856, 4.002877712838976976, 3.747395293195558847E-16 ) ) ;
#11829 = CARTESIAN_POINT ( 'NONE',  ( -10.00000000000000000, 0.000000000000000000, 0.000000000000000000 ) ) ;
#11830 = VERTEX_POINT ( 'NONE', #9727 ) ;
#11831 = DIRECTION ( 'NONE',  ( 0.000000000000000000, 0.000000000000000000, 1.000000000000000000 ) ) ;
#11832 = CYLINDRICAL_SURFACE ( 'NONE', #7502, 9.599999999999997868 ) ;
#11833 = CARTESIAN_POINT ( 'NONE',  ( 0.6279411196271856843, -4.781877258324073843, 10.00000000000000000 ) ) ;
#11834 = ADVANCED_FACE ( 'NONE', ( #8818 ), #423, .T. ) ;
#11835 = VECTOR ( 'NONE', #8347, 1000.000000000000000 ) ;
#11836 = CARTESIAN_POINT ( 'NONE',  ( -7.130211940009568927, -7.605417807865418212, 6.857782953271941950E-17 ) ) ;
#11837 = CARTESIAN_POINT ( 'NONE',  ( 0.000000000000000000, 21.76479567747241717, 7.432877647175279101 ) ) ;
#11838 = CARTESIAN_POINT ( 'NONE',  ( 3.000000000000000888, 13.79477846460795831, 18.40266524480593802 ) ) ;
#11839 = ORIENTED_EDGE ( 'NONE', *, *, #1685, .T. ) ;
#11840 = EDGE_CURVE ( 'NONE', #1170, #7842, #6880, .T. ) ;
#11841 = ORIENTED_EDGE ( 'NONE', *, *, #8380, .T. ) ;
#11842 = EDGE_LOOP ( 'NONE', ( #2271, #9604, #7289, #432 ) ) ;
#11843 = CARTESIAN_POINT ( 'NONE',  ( -12.04643853703213807, -0.2059847383341459892, 10.00000000000000000 ) ) ;
#11844 = CARTESIAN_POINT ( 'NONE',  ( 3.000000000000000888, 2.811977935938088535, -22.37663021667340857 ) ) ;
#11845 = CYLINDRICAL_SURFACE ( 'NONE', #9358, 19.99999999999999645 ) ;
#11846 = EDGE_CURVE ( 'NONE', #6939, #2895, #4341, .T. ) ;
#11847 = CARTESIAN_POINT ( 'NONE',  ( -8.409270314015810044, 2.833341551407462244, 3.747395293195558847E-16 ) ) ;
#11848 = DIRECTION ( 'NONE',  ( -1.000000000000000000, 0.000000000000000000, -0.000000000000000000 ) ) ;
#11849 = CARTESIAN_POINT ( 'NONE',  ( 0.000000000000000000, 0.3433949777334901476, -22.99643626497956461 ) ) ;
#11850 = ORIENTED_EDGE ( 'NONE', *, *, #6168, .F. ) ;
#11851 = ORIENTED_EDGE ( 'NONE', *, *, #3569, .F. ) ;
#11852 = EDGE_LOOP ( 'NONE', ( #6821, #96 ) ) ;
#11853 = CARTESIAN_POINT ( 'NONE',  ( 3.000000000000000888, -15.42759117534374447, -16.45023496161680754 ) ) ;
#11854 = DIRECTION ( 'NONE',  ( 0.000000000000000000, 0.000000000000000000, 1.000000000000000000 ) ) ;
#11855 = UNCERTAINTY_MEASURE_WITH_UNIT (LENGTH_MEASURE( 1.000000000000000082E-05 ), #8674, 'distance_accuracy_value', 'NONE');
#11856 = FACE_OUTER_BOUND ( 'NONE', #11741, .T. ) ;
#11857 = ORIENTED_EDGE ( 'NONE', *, *, #9886, .T. ) ;
#11858 = ADVANCED_FACE ( 'NONE', ( #6306 ), #5201, .T. ) ;
#11859 = DIRECTION ( 'NONE',  ( 1.000000000000000000, 0.000000000000000000, -0.000000000000000000 ) ) ;
#11860 = DIRECTION ( 'NONE',  ( -1.000000000000000000, -0.000000000000000000, -0.000000000000000000 ) ) ;
#11861 = CARTESIAN_POINT ( 'NONE',  ( 0.6279411196271849072, -4.781877258324066737, 6.857782953271941950E-17 ) ) ;
#11862 = DIRECTION ( 'NONE',  ( -1.000000000000000000, 0.000000000000000000, -0.000000000000000000 ) ) ;
#11863 = ORIENTED_EDGE ( 'NONE', *, *, #2288, .T. ) ;
#11864 = CARTESIAN_POINT ( 'NONE',  ( 3.000000000000000888, 0.000000000000000000, 0.000000000000000000 ) ) ;
#11865 = ORIENTED_EDGE ( 'NONE', *, *, #5328, .F. ) ;
#11866 = CIRCLE ( 'NONE', #2891, 3.500000000000000000 ) ;
#11867 = ORIENTED_EDGE ( 'NONE', *, *, #10575, .T. ) ;
#11868 = CARTESIAN_POINT ( 'NONE',  ( -0.9167995209625440234, 5.268308710424125074, 10.00000000000000000 ) ) ;
#11869 = ORIENTED_EDGE ( 'NONE', *, *, #2022, .T. ) ;
#11870 = FACE_OUTER_BOUND ( 'NONE', #11203, .T. ) ;
#11871 = ORIENTED_EDGE ( 'NONE', *, *, #5457, .F. ) ;
#11872 = CARTESIAN_POINT ( 'NONE',  ( 3.000000000000000888, 4.240409074144393387, -22.15038895030644639 ) ) ;
#11873 = CYLINDRICAL_SURFACE ( 'NONE', #3614, 24.80000000000000071 ) ;
#11874 = CARTESIAN_POINT ( 'NONE',  ( 5.027256439335601179, -9.798587832406491671, 10.00000000000000000 ) ) ;
#11875 = CARTESIAN_POINT ( 'NONE',  ( 3.000000000000000888, -9.039786367038983528, 21.14796121233193560 ) ) ;
#11876 = DIRECTION ( 'NONE',  ( 0.000000000000000000, 0.000000000000000000, 1.000000000000000000 ) ) ;
#11877 = VERTEX_POINT ( 'NONE', #8936 ) ;
#11878 = EDGE_LOOP ( 'NONE', ( #581, #7345, #5770, #2621 ) ) ;
#11879 = EDGE_CURVE ( 'NONE', #9193, #11632, #2193, .T. ) ;
#11880 = DIRECTION ( 'NONE',  ( 0.000000000000000000, -0.9135454576426046414, 0.4067366430757920481 ) ) ;
#11881 = ORIENTED_EDGE ( 'NONE', *, *, #11096, .F. ) ;
#11882 = CARTESIAN_POINT ( 'NONE',  ( 3.571029491936644540, 3.388293644658557646, 3.747395293195558847E-16 ) ) ;
#11883 = AXIS2_PLACEMENT_3D ( 'NONE', #11255, #7380, #157 ) ;
#11884 = EDGE_CURVE ( 'NONE', #2253, #1256, #2503, .T. ) ;
#11885 = CIRCLE ( 'NONE', #6801, 22.00000000000000000 ) ;
#11886 = CARTESIAN_POINT ( 'NONE',  ( 0.000000000000000000, 20.65684170206491999, 13.72351598154904195 ) ) ;
#11887 = ORIENTED_EDGE ( 'NONE', *, *, #11840, .T. ) ;
#11888 = DIRECTION ( 'NONE',  ( -1.000000000000000000, 0.000000000000000000, 0.000000000000000000 ) ) ;
#11889 = DIRECTION ( 'NONE',  ( -1.000000000000000000, -0.000000000000000000, 0.000000000000000000 ) ) ;
#11890 = DIRECTION ( 'NONE',  ( -1.000000000000000000, -0.000000000000000000, 0.000000000000000000 ) ) ;
#11891 = CARTESIAN_POINT ( 'NONE',  ( -5.542557460684662374, -4.854674288180239827, 10.00000000000000000 ) ) ;
#11892 = EDGE_CURVE ( 'NONE', #8778, #2132, #2981, .T. ) ;
#11893 = CARTESIAN_POINT ( 'NONE',  ( -5.125696908148159814, -9.212757455309411370, 6.857782953271941950E-17 ) ) ;
#11894 = DIRECTION ( 'NONE',  ( 0.000000000000000000, 0.000000000000000000, 1.000000000000000000 ) ) ;
#11895 = EDGE_CURVE ( 'NONE', #8200, #35, #11380, .T. ) ;
#11896 = CIRCLE ( 'NONE', #6620, 9.599999999999997868 ) ;
#11897 = CARTESIAN_POINT ( 'NONE',  ( 0.000000000000000000, 13.23915371906980631, -18.80635025205156907 ) ) ;
#11898 = VERTEX_POINT ( 'NONE', #4459 ) ;
#11899 = AXIS2_PLACEMENT_3D ( 'NONE', #10552, #5909, #2171 ) ;
#11900 = VERTEX_POINT ( 'NONE', #784 ) ;
#11901 = CARTESIAN_POINT ( 'NONE',  ( 7.019749797092301513, 12.16723183298456057, 10.00000000000000000 ) ) ;
#11902 = CIRCLE ( 'NONE', #764, 22.99900000000000233 ) ;
#11903 = AXIS2_PLACEMENT_3D ( 'NONE', #6535, #10211, #11254 ) ;
#11904 = DIRECTION ( 'NONE',  ( 0.000000000000000000, -0.9510565162951566398, 0.3090169943749381254 ) ) ;
#11905 = DIRECTION ( 'NONE',  ( 0.000000000000000000, 0.000000000000000000, -1.000000000000000000 ) ) ;
#11906 = CARTESIAN_POINT ( 'NONE',  ( -7.370305768634978882, 4.727533884956530486, 3.747395293195558847E-16 ) ) ;
#11907 = CARTESIAN_POINT ( 'NONE',  ( 3.000000000000000888, -19.29833442572367375, 11.67026512804540950 ) ) ;
#11908 = DIRECTION ( 'NONE',  ( -1.000000000000000000, -0.000000000000000000, -0.000000000000000000 ) ) ;
#11909 = EDGE_LOOP ( 'NONE', ( #3759, #5797, #3057, #5830 ) ) ;
#11910 = ORIENTED_EDGE ( 'NONE', *, *, #3540, .T. ) ;
#11911 = FACE_OUTER_BOUND ( 'NONE', #10613, .T. ) ;
#11912 = DIRECTION ( 'NONE',  ( -1.000000000000000000, -0.000000000000000000, 0.000000000000000000 ) ) ;
#11913 = CARTESIAN_POINT ( 'NONE',  ( 3.000000000000000888, 11.20082935824075321, 20.08719549084868561 ) ) ;
#11914 = CIRCLE ( 'NONE', #8413, 22.99899999999999878 ) ;
#11915 = EDGE_CURVE ( 'NONE', #9819, #9915, #9238, .T. ) ;
#11916 = DIRECTION ( 'NONE',  ( -1.000000000000000000, -0.000000000000000000, -0.000000000000000000 ) ) ;
#11917 = VECTOR ( 'NONE', #3034, 1000.000000000000000 ) ;
#11918 = CARTESIAN_POINT ( 'NONE',  ( 0.000000000000000000, 0.000000000000000000, 0.000000000000000000 ) ) ;
#11919 = CARTESIAN_POINT ( 'NONE',  ( 4.346347989803176937, 4.041826679702269942, 6.857782953271941950E-17 ) ) ;
#11920 = CARTESIAN_POINT ( 'NONE',  ( 3.000000000000000888, 13.72351598154897268, 20.65684170206495907 ) ) ;
#11921 = VERTEX_POINT ( 'NONE', #9966 ) ;
#11922 = DIRECTION ( 'NONE',  ( 0.000000000000000000, -0.9945218953682744001, 0.1045284632676437564 ) ) ;
#11923 = EDGE_CURVE ( 'NONE', #3460, #4090, #10805, .T. ) ;
#11924 = CIRCLE ( 'NONE', #10750, 9.599999999999997868 ) ;
#11925 = EDGE_LOOP ( 'NONE', ( #4988, #11384, #3102, #39 ) ) ;
#11926 = ORIENTED_EDGE ( 'NONE', *, *, #4074, .T. ) ;
#11927 = CIRCLE ( 'NONE', #5683, 9.599999999999996092 ) ;
#11928 = CARTESIAN_POINT ( 'NONE',  ( -0.1881845630465191765, -6.755137126427050553, 10.00000000000000000 ) ) ;
#11929 = EDGE_LOOP ( 'NONE', ( #10733, #4157, #5513, #6639 ) ) ;
#11930 = CARTESIAN_POINT ( 'NONE',  ( 1.499999999999999556, -3.623565124517271752, 24.53384959170456270 ) ) ;
#11931 = ORIENTED_EDGE ( 'NONE', *, *, #1649, .T. ) ;
#11932 = DIRECTION ( 'NONE',  ( -1.000000000000000000, 0.000000000000000000, 0.000000000000000000 ) ) ;
#11933 = LINE ( 'NONE', #8336, #4593 ) ;
#11934 = CARTESIAN_POINT ( 'NONE',  ( -6.825012239887744414, 1.243808647927287403, 10.00000000000000000 ) ) ;
#11935 = AXIS2_PLACEMENT_3D ( 'NONE', #8399, #7343, #5454 ) ;
#11936 = VECTOR ( 'NONE', #5244, 1000.000000000000000 ) ;
#11937 = DIRECTION ( 'NONE',  ( 0.000000000000000000, 0.9135454576425990902, 0.4067366430758041496 ) ) ;
#11938 = VECTOR ( 'NONE', #7027, 1000.000000000000000 ) ;
#11939 = DIRECTION ( 'NONE',  ( -1.000000000000000000, 0.000000000000000000, 0.000000000000000000 ) ) ;
#11940 = ORIENTED_EDGE ( 'NONE', *, *, #1003, .F. ) ;
#11941 = FACE_OUTER_BOUND ( 'NONE', #1684, .T. ) ;
#11942 = ORIENTED_EDGE ( 'NONE', *, *, #3454, .T. ) ;
#11943 = CARTESIAN_POINT ( 'NONE',  ( 0.5697670706242773386, -3.781298318517893442, 3.747395293195558847E-16 ) ) ;
#11944 = CIRCLE ( 'NONE', #5081, 22.99899999999999878 ) ;
#11945 = CYLINDRICAL_SURFACE ( 'NONE', #1087, 24.80000000000000071 ) ;
#11946 = ORIENTED_EDGE ( 'NONE', *, *, #11726, .T. ) ;
#11947 = AXIS2_PLACEMENT_3D ( 'NONE', #7295, #2479, #11894 ) ;
#11948 = CARTESIAN_POINT ( 'NONE',  ( 0.000000000000000000, 0.000000000000000000, 4.000000000000000000 ) ) ;
#11949 = CARTESIAN_POINT ( 'NONE',  ( 3.000000000000000888, -5.117118920208643118, 22.42251312757878168 ) ) ;
#11950 = FACE_OUTER_BOUND ( 'NONE', #11734, .T. ) ;
#11951 = DIRECTION ( 'NONE',  ( 0.000000000000000000, 0.000000000000000000, 1.000000000000000000 ) ) ;
#11952 = CARTESIAN_POINT ( 'NONE',  ( -0.2556890074706221205, -7.756263830888991961, 6.857782953271941950E-17 ) ) ;
#11953 = CARTESIAN_POINT ( 'NONE',  ( 0.000000000000000000, -16.85990652506889376, -15.64281154287614584 ) ) ;
#11954 = AXIS2_PLACEMENT_3D ( 'NONE', #5839, #261, #7543 ) ;
#11955 = DIRECTION ( 'NONE',  ( -1.000000000000000000, -0.000000000000000000, 0.000000000000000000 ) ) ;
#11956 = EDGE_CURVE ( 'NONE', #7635, #10066, #10217, .T. ) ;
#11957 = VECTOR ( 'NONE', #6122, 1000.000000000000000 ) ;
#11958 = ORIENTED_EDGE ( 'NONE', *, *, #227, .F. ) ;
#11959 = EDGE_LOOP ( 'NONE', ( #9900, #5786, #11988, #10172 ) ) ;
#11960 = ORIENTED_EDGE ( 'NONE', *, *, #3011, .T. ) ;
#11961 = EDGE_CURVE ( 'NONE', #7191, #5600, #2987, .T. ) ;
#11962 = CARTESIAN_POINT ( 'NONE',  ( 10.44364468045616157, 9.157203537818526584, 10.00000000000000000 ) ) ;
#11963 = EDGE_CURVE ( 'NONE', #9081, #862, #7262, .T. ) ;
#11964 = DIRECTION ( 'NONE',  ( -1.000000000000000000, 0.000000000000000000, 0.000000000000000000 ) ) ;
#11965 = FACE_OUTER_BOUND ( 'NONE', #715, .T. ) ;
#11966 = EDGE_CURVE ( 'NONE', #6502, #6248, #2793, .T. ) ;
#11967 = CARTESIAN_POINT ( 'NONE',  ( 7.261170810407326037, -1.543028577657243439, 3.747395293195558847E-16 ) ) ;
#11968 = DIRECTION ( 'NONE',  ( -1.000000000000000000, 0.000000000000000000, 0.000000000000000000 ) ) ;
#11969 = ORIENTED_EDGE ( 'NONE', *, *, #3703, .T. ) ;
#11970 = DIRECTION ( 'NONE',  ( -1.000000000000000000, -0.000000000000000000, 0.000000000000000000 ) ) ;
#11971 = ORIENTED_EDGE ( 'NONE', *, *, #7333, .F. ) ;
#11972 = VERTEX_POINT ( 'NONE', #607 ) ;
#11973 = ORIENTED_EDGE ( 'NONE', *, *, #9617, .F. ) ;
#11974 = EDGE_CURVE ( 'NONE', #5828, #12032, #2003, .T. ) ;
#11975 = DIRECTION ( 'NONE',  ( 0.000000000000000000, 0.9781476007338049117, 0.2079116908177629230 ) ) ;
#11976 = AXIS2_PLACEMENT_3D ( 'NONE', #11735, #7073, #11797 ) ;
#11977 = VECTOR ( 'NONE', #3642, 1000.000000000000000 ) ;
#11978 = FACE_OUTER_BOUND ( 'NONE', #7056, .T. ) ;
#11979 = CARTESIAN_POINT ( 'NONE',  ( 3.000000000000000888, -24.75110766671653195, 1.556492618230561842 ) ) ;
#11980 = CARTESIAN_POINT ( 'NONE',  ( 3.000000000000000888, -11.20082935824061110, -20.08719549084876732 ) ) ;
#11981 = AXIS2_PLACEMENT_3D ( 'NONE', #3490, #7200, #8193 ) ;
#11982 = FACE_OUTER_BOUND ( 'NONE', #11493, .T. ) ;
#11983 = DIRECTION ( 'NONE',  ( -1.000000000000000000, -0.000000000000000000, 0.000000000000000000 ) ) ;
#11984 = CARTESIAN_POINT ( 'NONE',  ( 5.531377455021717182, -0.3672033614207537711, 6.857782953271941950E-17 ) ) ;
#11985 = EDGE_CURVE ( 'NONE', #11830, #10120, #2596, .T. ) ;
#11986 = CARTESIAN_POINT ( 'NONE',  ( 0.000000000000000000, 6.168200451486084646, -24.02068490260606026 ) ) ;
#11987 = EDGE_LOOP ( 'NONE', ( #8585, #3814, #997, #9301 ) ) ;
#11988 = ORIENTED_EDGE ( 'NONE', *, *, #8754, .T. ) ;
#11989 = DIRECTION ( 'NONE',  ( -1.000000000000000000, 0.000000000000000000, 0.000000000000000000 ) ) ;
#11990 = ORIENTED_EDGE ( 'NONE', *, *, #11963, .T. ) ;
#11991 = EDGE_CURVE ( 'NONE', #10351, #4929, #6503, .T. ) ;
#11992 = VECTOR ( 'NONE', #697, 1000.000000000000000 ) ;
#11993 = VERTEX_POINT ( 'NONE', #8135 ) ;
#11994 = CARTESIAN_POINT ( 'NONE',  ( -5.359287035704432434, 6.724520318541068242, 10.00000000000000000 ) ) ;
#11995 = ORIENTED_EDGE ( 'NONE', *, *, #12079, .T. ) ;
#11996 = DIRECTION ( 'NONE',  ( -1.000000000000000000, -0.000000000000000000, -0.000000000000000000 ) ) ;
#11997 = ORIENTED_EDGE ( 'NONE', *, *, #2622, .F. ) ;
#11998 = CYLINDRICAL_SURFACE ( 'NONE', #4952, 9.599999999999997868 ) ;
#11999 = EDGE_CURVE ( 'NONE', #1084, #5065, #4754, .T. ) ;
#12000 =( REPRESENTATION_RELATIONSHIP ('NONE','NONE', #8743, #8353 ) REPRESENTATION_RELATIONSHIP_WITH_TRANSFORMATION ( #1397 )SHAPE_REPRESENTATION_RELATIONSHIP( ) );
#12001 = DIRECTION ( 'NONE',  ( 0.000000000000000000, 0.000000000000000000, 1.000000000000000000 ) ) ;
#12002 = CARTESIAN_POINT ( 'NONE',  ( -15.18624859168667562, -5.715447929355453205, 6.857782953271941950E-17 ) ) ;
#12003 = AXIS2_PLACEMENT_3D ( 'NONE', #2643, #3566, #6255 ) ;
#12004 = CARTESIAN_POINT ( 'NONE',  ( 3.000000000000000888, -6.532525787311115550, 21.58580335785674365 ) ) ;
#12005 = DIRECTION ( 'NONE',  ( -1.000000000000000000, 0.000000000000000000, 0.000000000000000000 ) ) ;
#12006 = ORIENTED_EDGE ( 'NONE', *, *, #1414, .F. ) ;
#12007 = CARTESIAN_POINT ( 'NONE',  ( 3.000000000000000888, -7.402892494506437160, 21.30300407174360444 ) ) ;
#12008 = VERTEX_POINT ( 'NONE', #10949 ) ;
#12009 = CARTESIAN_POINT ( 'NONE',  ( 6.723006375386860967, 3.907299473125124489, 3.747395293195558847E-16 ) ) ;
#12010 = AXIS2_PLACEMENT_3D ( 'NONE', #10043, #1664, #12001 ) ;
#12011 = CYLINDRICAL_SURFACE ( 'NONE', #7323, 9.599999999999997868 ) ;
#12012 = EDGE_CURVE ( 'NONE', #3450, #4165, #161, .T. ) ;
#12013 = DIRECTION ( 'NONE',  ( -1.000000000000000000, 0.000000000000000000, 0.000000000000000000 ) ) ;
#12014 = DIRECTION ( 'NONE',  ( -1.000000000000000000, -0.000000000000000000, 0.000000000000000000 ) ) ;
#12015 = DIRECTION ( 'NONE',  ( -1.000000000000000000, -0.000000000000000000, 0.000000000000000000 ) ) ;
#12016 = CARTESIAN_POINT ( 'NONE',  ( 3.000000000000000888, 20.93895013827581764, 13.28910708463135570 ) ) ;
#12017 = CARTESIAN_POINT ( 'NONE',  ( 6.242895496888662521, -5.302832405932363713, 6.857782953271941950E-17 ) ) ;
#12018 = DIRECTION ( 'NONE',  ( 0.000000000000000000, 0.000000000000000000, 1.000000000000000000 ) ) ;
#12019 = VERTEX_POINT ( 'NONE', #6582 ) ;
#12020 = ORIENTED_EDGE ( 'NONE', *, *, #556, .F. ) ;
#12021 = ORIENTED_EDGE ( 'NONE', *, *, #11233, .T. ) ;
#12022 = CARTESIAN_POINT ( 'NONE',  ( 0.000000000000000000, 21.14796121233209192, -9.039786367038628256 ) ) ;
#12023 = CARTESIAN_POINT ( 'NONE',  ( -4.622662292628551661, -8.344572748942844953, 10.00000000000000000 ) ) ;
#12024 = DIRECTION ( 'NONE',  ( -1.000000000000000000, -0.000000000000000000, -0.000000000000000000 ) ) ;
#12025 = CYLINDRICAL_SURFACE ( 'NONE', #10730, 9.599999999999997868 ) ;
#12026 = CIRCLE ( 'NONE', #6173, 9.599999999999997868 ) ;
#12027 = CARTESIAN_POINT ( 'NONE',  ( 0.6578947103914138950, -9.792230064638470566, 3.747395293195558847E-16 ) ) ;
#12028 = CARTESIAN_POINT ( 'NONE',  ( 1.631735293711819246, 4.895207720155139164, 3.747395293195558847E-16 ) ) ;
#12029 = DIRECTION ( 'NONE',  ( -1.000000000000000000, 0.000000000000000000, 0.000000000000000000 ) ) ;
#12030 = EDGE_LOOP ( 'NONE', ( #4883, #10964, #9107, #11156 ) ) ;
#12031 = EDGE_CURVE ( 'NONE', #8566, #5393, #10997, .T. ) ;
#12032 = VERTEX_POINT ( 'NONE', #8432 ) ;
#12033 = VECTOR ( 'NONE', #1418, 1000.000000000000000 ) ;
#12034 = EDGE_CURVE ( 'NONE', #11531, #9193, #11115, .T. ) ;
#12035 = ORIENTED_EDGE ( 'NONE', *, *, #5161, .F. ) ;
#12036 = DIRECTION ( 'NONE',  ( 1.000000000000000000, 0.000000000000000000, 0.000000000000000000 ) ) ;
#12037 = CARTESIAN_POINT ( 'NONE',  ( 0.000000000000000000, 0.000000000000000000, 1.000000000000000000 ) ) ;
#12038 = DIRECTION ( 'NONE',  ( 1.000000000000000000, 0.000000000000000000, 0.000000000000000000 ) ) ;
#12039 = CARTESIAN_POINT ( 'NONE',  ( 3.000000000000000888, -15.80756504416678432, -19.10918332567973721 ) ) ;
#12040 = DIRECTION ( 'NONE',  ( 0.000000000000000000, 0.000000000000000000, 1.000000000000000000 ) ) ;
#12041 = AXIS2_PLACEMENT_3D ( 'NONE', #420, #3063, #11443 ) ;
#12042 = CARTESIAN_POINT ( 'NONE',  ( 15.00667705184753764, -6.512453894250635145, 3.747395293195558847E-16 ) ) ;
#12043 = CARTESIAN_POINT ( 'NONE',  ( 7.449730884303669143, -3.679036338562942543, 6.857782953271941950E-17 ) ) ;
#12044 = EDGE_CURVE ( 'NONE', #12008, #9035, #4553, .T. ) ;
#12045 = EDGE_CURVE ( 'NONE', #2082, #5009, #9431, .T. ) ;
#12046 = CARTESIAN_POINT ( 'NONE',  ( 3.000000000000000888, 0.000000000000000000, 0.000000000000000000 ) ) ;
#12047 = EDGE_LOOP ( 'NONE', ( #1819, #5810, #10800, #172 ) ) ;
#12048 = ORIENTED_EDGE ( 'NONE', *, *, #10093, .T. ) ;
#12049 = DIRECTION ( 'NONE',  ( -1.000000000000000000, 0.000000000000000000, 0.000000000000000000 ) ) ;
#12050 = VERTEX_POINT ( 'NONE', #7304 ) ;
#12051 = ORIENTED_EDGE ( 'NONE', *, *, #1836, .F. ) ;
#12052 = CARTESIAN_POINT ( 'NONE',  ( 5.211919109253434712, 5.981019939437272726, 10.00000000000000000 ) ) ;
#12053 = ORIENTED_EDGE ( 'NONE', *, *, #7677, .F. ) ;
#12054 = CARTESIAN_POINT ( 'NONE',  ( 0.000000000000000000, -17.31945870441136748, -15.13242714128137401 ) ) ;
#12055 = VERTEX_POINT ( 'NONE', #3714 ) ;
#12056 = CYLINDRICAL_SURFACE ( 'NONE', #1818, 19.00000000000000000 ) ;
#12057 = CARTESIAN_POINT ( 'NONE',  ( 3.000000000000000888, 20.78471918669872665, -8.753070780932940664 ) ) ;
#12058 = CARTESIAN_POINT ( 'NONE',  ( 14.52660474336492236, -9.366294961249355566, 6.857782953271941950E-17 ) ) ;
#12059 = CARTESIAN_POINT ( 'NONE',  ( 3.000000000000000888, 16.45023496161665122, 15.42759117534391322 ) ) ;
#12060 = CARTESIAN_POINT ( 'NONE',  ( 0.000000000000000000, 0.000000000000000000, 0.000000000000000000 ) ) ;
#12061 = ORIENTED_EDGE ( 'NONE', *, *, #1157, .T. ) ;
#12062 = ORIENTED_EDGE ( 'NONE', *, *, #7018, .T. ) ;
#12063 = DIRECTION ( 'NONE',  ( -1.000000000000000000, 0.000000000000000000, 0.000000000000000000 ) ) ;
#12064 = EDGE_LOOP ( 'NONE', ( #1319, #10511, #1662, #2707 ) ) ;
#12065 = CARTESIAN_POINT ( 'NONE',  ( -5.704017324792769905, 1.489539271746818772, 3.747395293195558847E-16 ) ) ;
#12066 = CARTESIAN_POINT ( 'NONE',  ( 3.000000000000000888, 22.42251312757886339, -5.117118920208268307 ) ) ;
#12067 =( LENGTH_UNIT ( ) NAMED_UNIT ( * ) SI_UNIT ( .MILLI., .METRE. ) );
#12068 = CIRCLE ( 'NONE', #1915, 22.99900000000000233 ) ;
#12069 = CARTESIAN_POINT ( 'NONE',  ( 0.000000000000000000, -21.58580335785681115, 6.532525787310899723 ) ) ;
#12070 = DIRECTION ( 'NONE',  ( 0.000000000000000000, 0.9781476007338048007, 0.2079116908177630618 ) ) ;
#12071 = FACE_OUTER_BOUND ( 'NONE', #10658, .T. ) ;
#12072 = EDGE_CURVE ( 'NONE', #5151, #3060, #1041, .T. ) ;
#12073 = CARTESIAN_POINT ( 'NONE',  ( -3.764233030011069125, -6.516208816467297105, 6.857782953271941950E-17 ) ) ;
#12074 = FACE_OUTER_BOUND ( 'NONE', #5197, .T. ) ;
#12075 = DIRECTION ( 'NONE',  ( 0.000000000000000000, 0.000000000000000000, 1.000000000000000000 ) ) ;
#12076 = ORIENTED_EDGE ( 'NONE', *, *, #8191, .T. ) ;
#12077 = VECTOR ( 'NONE', #6591, 1000.000000000000000 ) ;
#12078 = ORIENTED_EDGE ( 'NONE', *, *, #11072, .F. ) ;
#12079 = EDGE_CURVE ( 'NONE', #8706, #3600, #898, .T. ) ;
#12080 = ORIENTED_EDGE ( 'NONE', *, *, #4810, .F. ) ;
#12081 = DIRECTION ( 'NONE',  ( -1.000000000000000000, -0.000000000000000000, -0.000000000000000000 ) ) ;
#12082 = CARTESIAN_POINT ( 'NONE',  ( 8.800885721068839374, 6.316044917328129671, 10.00000000000000000 ) ) ;
#12083 = LINE ( 'NONE', #1869, #11560 ) ;
#12084 = CARTESIAN_POINT ( 'NONE',  ( 3.000000000000000888, 0.000000000000000000, 0.000000000000000000 ) ) ;
#12085 = CARTESIAN_POINT ( 'NONE',  ( 1.499999999999999556, -9.128825345753185161, 23.05871956130119571 ) ) ;
#12086 = CARTESIAN_POINT ( 'NONE',  ( -4.622662292628548997, -8.344572748942098883, 3.747395293195558847E-16 ) ) ;
#12087 = VECTOR ( 'NONE', #3235, 1000.000000000000000 ) ;
#12088 = AXIS2_PLACEMENT_3D ( 'NONE', #4013, #7738, #2794 ) ;
#12089 = CARTESIAN_POINT ( 'NONE',  ( 0.000000000000000000, 0.000000000000000000, 3.000000000000000000 ) ) ;
#12090 = DIRECTION ( 'NONE',  ( 0.000000000000000000, 0.000000000000000000, 1.000000000000000000 ) ) ;
#12091 = VERTEX_POINT ( 'NONE', #10261 ) ;
#12092 = ORIENTED_EDGE ( 'NONE', *, *, #7934, .T. ) ;
#12093 = CARTESIAN_POINT ( 'NONE',  ( 3.000000000000000888, -22.42251312757876036, -5.117118920208720390 ) ) ;
#12094 = VECTOR ( 'NONE', #4568, 1000.000000000000000 ) ;
#12095 = LINE ( 'NONE', #2741, #8237 ) ;
#12096 = CARTESIAN_POINT ( 'NONE',  ( 0.000000000000000000, -5.135568396240178579, 21.96011696265489377 ) ) ;
#12097 = LINE ( 'NONE', #2007, #12077 ) ;
#12098 = DIRECTION ( 'NONE',  ( 0.000000000000000000, -0.4067366430757887730, -0.9135454576426059736 ) ) ;
#12099 = CARTESIAN_POINT ( 'NONE',  ( 12.88139461472923841, -9.891864711284155121, 3.747395293195558847E-16 ) ) ;
#12100 = CARTESIAN_POINT ( 'NONE',  ( -2.570438583093345386, 5.934334910739564428, 6.857782953271941950E-17 ) ) ;
#12101 = VECTOR ( 'NONE', #3430, 1000.000000000000000 ) ;
#12102 = AXIS2_PLACEMENT_3D ( 'NONE', #5925, #9474, #1090 ) ;
#12103 = VECTOR ( 'NONE', #2875, 1000.000000000000000 ) ;
#12104 = DIRECTION ( 'NONE',  ( 1.000000000000000000, 0.000000000000000000, 0.000000000000000000 ) ) ;
#12105 = EDGE_CURVE ( 'NONE', #2327, #730, #1747, .T. ) ;
#12106 = ORIENTED_EDGE ( 'NONE', *, *, #9518, .T. ) ;
#12107 = ORIENTED_EDGE ( 'NONE', *, *, #5237, .F. ) ;
#12108 = DIRECTION ( 'NONE',  ( -1.000000000000000000, 0.000000000000000000, 0.000000000000000000 ) ) ;
#12109 = ORIENTED_EDGE ( 'NONE', *, *, #1063, .F. ) ;
#12110 = ORIENTED_EDGE ( 'NONE', *, *, #5107, .F. ) ;
#12111 = CARTESIAN_POINT ( 'NONE',  ( 4.516389116325776776, 1.247036727255508737, 10.00000000000000000 ) ) ;
#12112 = EDGE_CURVE ( 'NONE', #2984, #8511, #2799, .T. ) ;
#12113 = FACE_OUTER_BOUND ( 'NONE', #8048, .T. ) ;
#12114 = ORIENTED_EDGE ( 'NONE', *, *, #3856, .F. ) ;
#12115 = ADVANCED_FACE ( 'NONE', ( #5554 ), #4575, .T. ) ;
#12116 = CIRCLE ( 'NONE', #4700, 24.80000000000000071 ) ;
#12117 = ORIENTED_EDGE ( 'NONE', *, *, #4525, .F. ) ;
#12118 = NEXT_ASSEMBLY_USAGE_OCCURRENCE ( 'NAUO1', ' ', ' ', #8151, #10317, $ ) ;
#12119 = NEXT_ASSEMBLY_USAGE_OCCURRENCE ( 'NAUO2', ' ', ' ', #8151, #10691, $ ) ;
#12120 = NEXT_ASSEMBLY_USAGE_OCCURRENCE ( 'NAUO3', ' ', ' ', #8151, #9054, $ ) ;
#12121 = NEXT_ASSEMBLY_USAGE_OCCURRENCE ( 'NAUO4', ' ', ' ', #8151, #9427, $ ) ;
#12122 = NEXT_ASSEMBLY_USAGE_OCCURRENCE ( 'NAUO5', ' ', ' ', #8151, #5612, $ ) ;
#12123 = NEXT_ASSEMBLY_USAGE_OCCURRENCE ( 'NAUO6', ' ', ' ', #8151, #9275, $ ) ;
ENDSEC;
END-ISO-10303-21;
